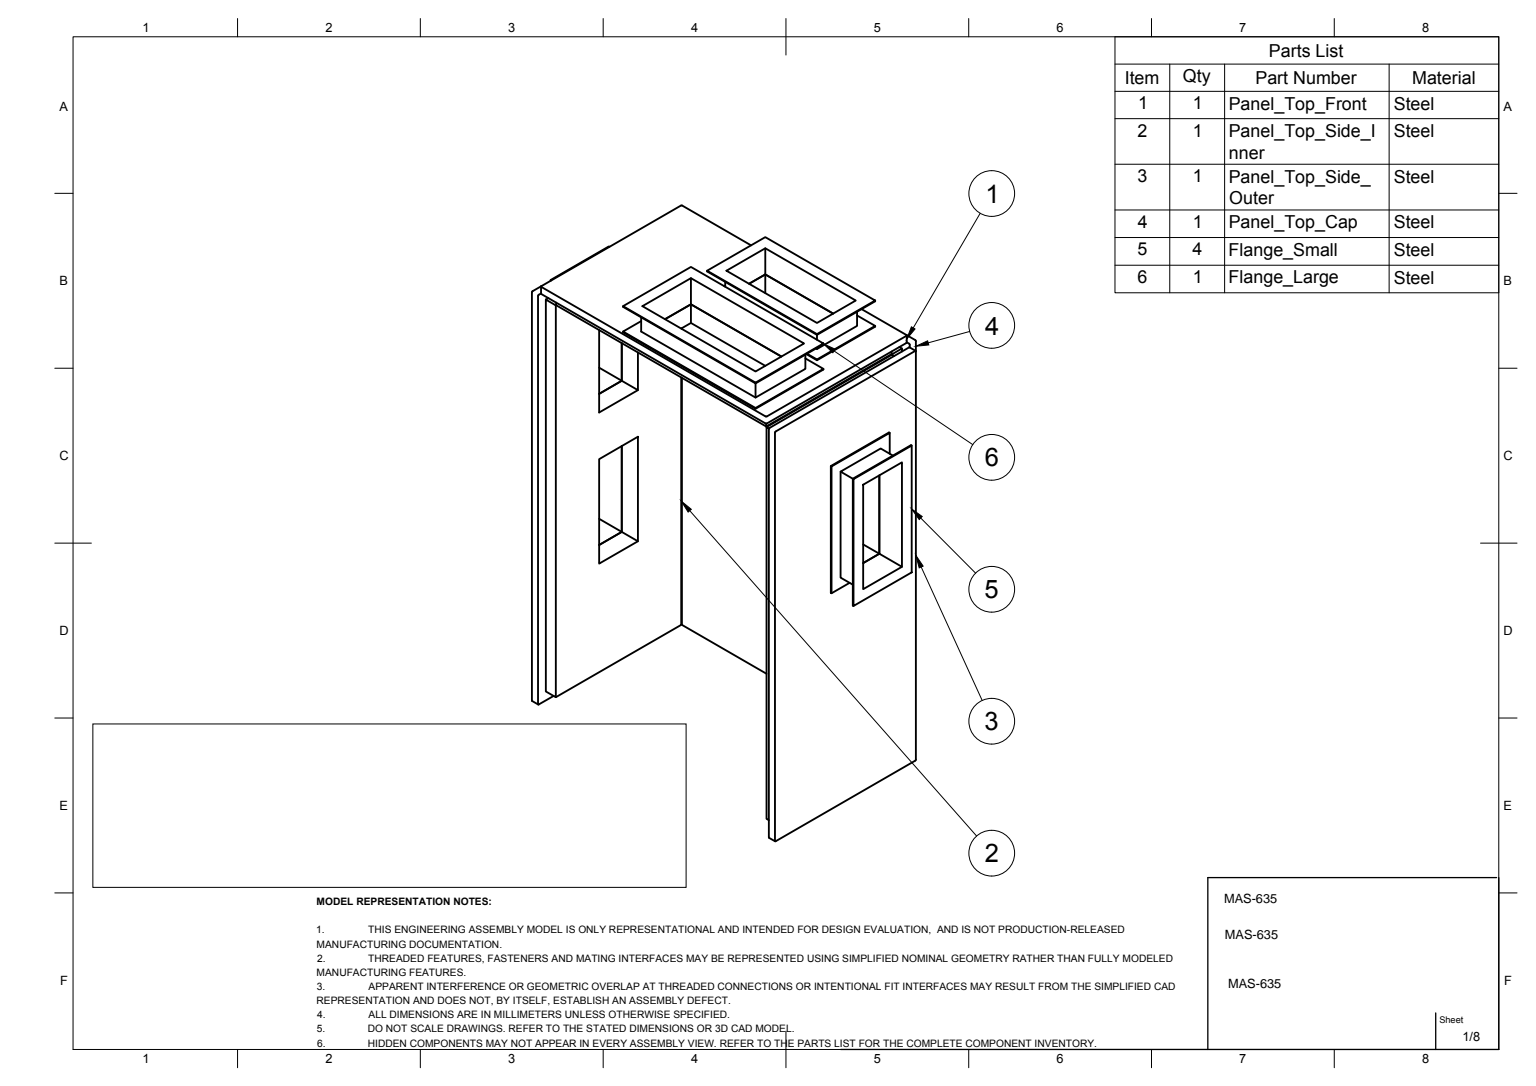
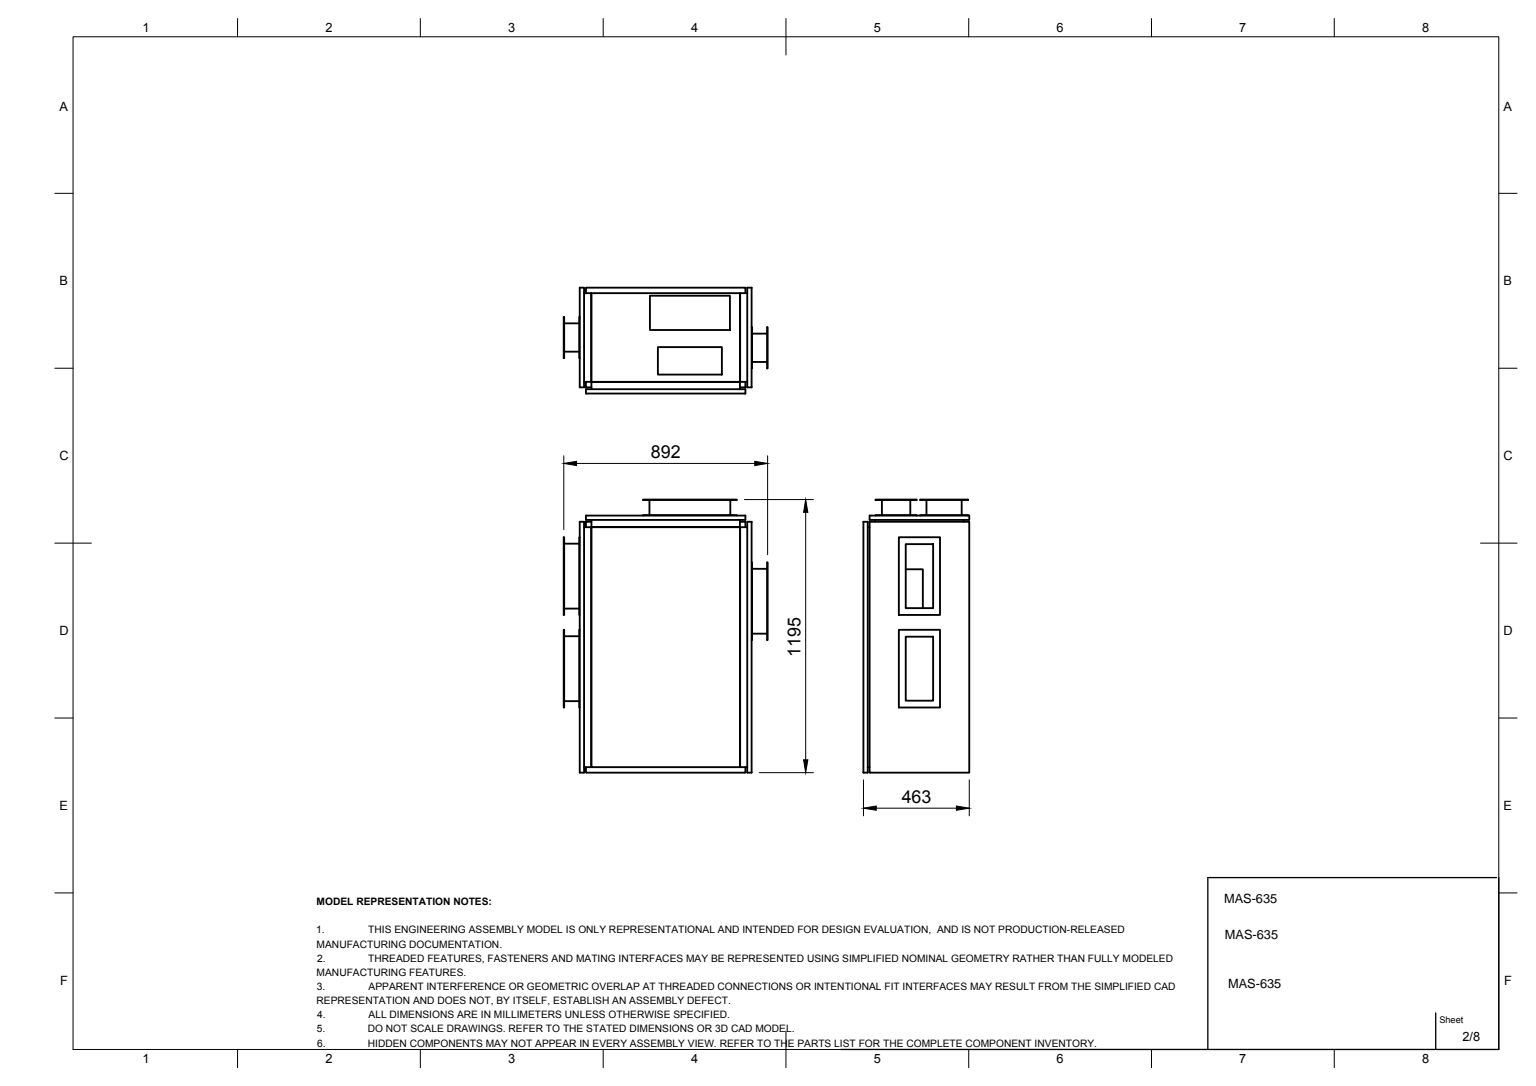
ISO-10303-21;
HEADER;
FILE_DESCRIPTION((''),'2;1');
FILE_NAME('MAS-635','2026-10-09T12:34:24-07:00',(''),(''),'','','');
FILE_SCHEMA (('AUTOMOTIVE_DESIGN { 1 0 10303 214 3 1 1 }'));
ENDSEC;
DATA;
#10 = MECHANICAL_DESIGN_GEOMETRIC_PRESENTATION_REPRESENTATION('',(#59,#60,
#61,#62,#63,#64),#3759) ;
#11 = ITEM_DEFINED_TRANSFORMATION($,$,#2337,#2495) ;
#12 = ITEM_DEFINED_TRANSFORMATION($,$,#2369,#2496) ;
#13 = ITEM_DEFINED_TRANSFORMATION($,$,#2401,#2497) ;
#14 = ITEM_DEFINED_TRANSFORMATION($,$,#2429,#2498) ;
#15 = ITEM_DEFINED_TRANSFORMATION($,$,#2474,#2499) ;
#16 = ITEM_DEFINED_TRANSFORMATION($,$,#2453,#2500) ;
#17 = ITEM_DEFINED_TRANSFORMATION($,$,#2474,#2501) ;
#18 = ITEM_DEFINED_TRANSFORMATION($,$,#2474,#2502) ;
#19 = ITEM_DEFINED_TRANSFORMATION($,$,#2474,#2503) ;
#20 = (
REPRESENTATION_RELATIONSHIP($,$,#3788,#3787)
REPRESENTATION_RELATIONSHIP_WITH_TRANSFORMATION(#11)
SHAPE_REPRESENTATION_RELATIONSHIP()
) ;
#21 = (
REPRESENTATION_RELATIONSHIP($,$,#3789,#3787)
REPRESENTATION_RELATIONSHIP_WITH_TRANSFORMATION(#12)
SHAPE_REPRESENTATION_RELATIONSHIP()
) ;
#22 = (
REPRESENTATION_RELATIONSHIP($,$,#3790,#3787)
REPRESENTATION_RELATIONSHIP_WITH_TRANSFORMATION(#13)
SHAPE_REPRESENTATION_RELATIONSHIP()
) ;
#23 = (
REPRESENTATION_RELATIONSHIP($,$,#3791,#3787)
REPRESENTATION_RELATIONSHIP_WITH_TRANSFORMATION(#14)
SHAPE_REPRESENTATION_RELATIONSHIP()
) ;
#24 = (
REPRESENTATION_RELATIONSHIP($,$,#3793,#3787)
REPRESENTATION_RELATIONSHIP_WITH_TRANSFORMATION(#15)
SHAPE_REPRESENTATION_RELATIONSHIP()
) ;
#25 = (
REPRESENTATION_RELATIONSHIP($,$,#3792,#3787)
REPRESENTATION_RELATIONSHIP_WITH_TRANSFORMATION(#16)
SHAPE_REPRESENTATION_RELATIONSHIP()
) ;
#26 = (
REPRESENTATION_RELATIONSHIP($,$,#3793,#3787)
REPRESENTATION_RELATIONSHIP_WITH_TRANSFORMATION(#17)
SHAPE_REPRESENTATION_RELATIONSHIP()
) ;
#27 = (
REPRESENTATION_RELATIONSHIP($,$,#3793,#3787)
REPRESENTATION_RELATIONSHIP_WITH_TRANSFORMATION(#18)
SHAPE_REPRESENTATION_RELATIONSHIP()
) ;
#28 = (
REPRESENTATION_RELATIONSHIP($,$,#3793,#3787)
REPRESENTATION_RELATIONSHIP_WITH_TRANSFORMATION(#19)
SHAPE_REPRESENTATION_RELATIONSHIP()
) ;
#29 = CONTEXT_DEPENDENT_SHAPE_REPRESENTATION(#20,#3778) ;
#30 = CONTEXT_DEPENDENT_SHAPE_REPRESENTATION(#21,#3779) ;
#31 = CONTEXT_DEPENDENT_SHAPE_REPRESENTATION(#22,#3780) ;
#32 = CONTEXT_DEPENDENT_SHAPE_REPRESENTATION(#23,#3781) ;
#33 = CONTEXT_DEPENDENT_SHAPE_REPRESENTATION(#24,#3782) ;
#34 = CONTEXT_DEPENDENT_SHAPE_REPRESENTATION(#25,#3783) ;
#35 = CONTEXT_DEPENDENT_SHAPE_REPRESENTATION(#26,#3784) ;
#36 = CONTEXT_DEPENDENT_SHAPE_REPRESENTATION(#27,#3785) ;
#37 = CONTEXT_DEPENDENT_SHAPE_REPRESENTATION(#28,#3786) ;
#38 = NEXT_ASSEMBLY_USAGE_OCCURRENCE('Panel_Top_Front:1',
'Panel_Top_Front:1','Panel_Top_Front:1',#3795,#3796,'Panel_Top_Front:1') ;
#39 = NEXT_ASSEMBLY_USAGE_OCCURRENCE('Panel_Top_Side_Inner:1',
'Panel_Top_Side_Inner:1','Panel_Top_Side_Inner:1',#3795,#3797,
'Panel_Top_Side_Inner:1') ;
#40 = NEXT_ASSEMBLY_USAGE_OCCURRENCE('Panel_Top_Side_Outer:1',
'Panel_Top_Side_Outer:1','Panel_Top_Side_Outer:1',#3795,#3798,
'Panel_Top_Side_Outer:1') ;
#41 = NEXT_ASSEMBLY_USAGE_OCCURRENCE('Panel_Top_Cap:1','Panel_Top_Cap:1',
'Panel_Top_Cap:1',#3795,#3799,'Panel_Top_Cap:1') ;
#42 = NEXT_ASSEMBLY_USAGE_OCCURRENCE('Flange_Small:1','Flange_Small:1',
'Flange_Small:1',#3795,#3801,'Flange_Small:1') ;
#43 = NEXT_ASSEMBLY_USAGE_OCCURRENCE('Flange_Large:1','Flange_Large:1',
'Flange_Large:1',#3795,#3800,'Flange_Large:1') ;
#44 = NEXT_ASSEMBLY_USAGE_OCCURRENCE('Flange_Small:2','Flange_Small:2',
'Flange_Small:2',#3795,#3801,'Flange_Small:2') ;
#45 = NEXT_ASSEMBLY_USAGE_OCCURRENCE('Flange_Small:3','Flange_Small:3',
'Flange_Small:3',#3795,#3801,'Flange_Small:3') ;
#46 = NEXT_ASSEMBLY_USAGE_OCCURRENCE('Flange_Small:4','Flange_Small:4',
'Flange_Small:4',#3795,#3801,'Flange_Small:4') ;
#47 = SHAPE_REPRESENTATION_RELATIONSHIP('SRR','None',#3788,#53) ;
#48 = SHAPE_REPRESENTATION_RELATIONSHIP('SRR','None',#3789,#54) ;
#49 = SHAPE_REPRESENTATION_RELATIONSHIP('SRR','None',#3790,#55) ;
#50 = SHAPE_REPRESENTATION_RELATIONSHIP('SRR','None',#3791,#56) ;
#51 = SHAPE_REPRESENTATION_RELATIONSHIP('SRR','None',#3792,#57) ;
#52 = SHAPE_REPRESENTATION_RELATIONSHIP('SRR','None',#3793,#58) ;
#53 = ADVANCED_BREP_SHAPE_REPRESENTATION('',(#65),#3753) ;
#54 = ADVANCED_BREP_SHAPE_REPRESENTATION('',(#66),#3754) ;
#55 = ADVANCED_BREP_SHAPE_REPRESENTATION('',(#67),#3755) ;
#56 = ADVANCED_BREP_SHAPE_REPRESENTATION('',(#68),#3756) ;
#57 = ADVANCED_BREP_SHAPE_REPRESENTATION('',(#69),#3757) ;
#58 = ADVANCED_BREP_SHAPE_REPRESENTATION('',(#70),#3758) ;
#59 = STYLED_ITEM('',(#3827),#65) ;
#60 = STYLED_ITEM('',(#3827),#66) ;
#61 = STYLED_ITEM('',(#3827),#67) ;
#62 = STYLED_ITEM('',(#3827),#68) ;
#63 = STYLED_ITEM('',(#3827),#69) ;
#64 = STYLED_ITEM('',(#3827),#70) ;
#65 = MANIFOLD_SOLID_BREP('Body1',#2263) ;
#66 = MANIFOLD_SOLID_BREP('Body1',#2264) ;
#67 = MANIFOLD_SOLID_BREP('Body1',#2265) ;
#68 = MANIFOLD_SOLID_BREP('Body1',#2266) ;
#69 = MANIFOLD_SOLID_BREP('Body1',#2267) ;
#70 = MANIFOLD_SOLID_BREP('Body1',#2268) ;
#71 = CYLINDRICAL_SURFACE('',#2357,0.2) ;
#72 = CYLINDRICAL_SURFACE('',#2358,0.2) ;
#73 = CYLINDRICAL_SURFACE('',#2359,0.2) ;
#74 = CYLINDRICAL_SURFACE('',#2360,0.2) ;
#75 = CYLINDRICAL_SURFACE('',#2389,0.2) ;
#76 = CYLINDRICAL_SURFACE('',#2390,0.2) ;
#77 = CYLINDRICAL_SURFACE('',#2391,0.2) ;
#78 = CYLINDRICAL_SURFACE('',#2392,0.2) ;
#79 = CYLINDRICAL_SURFACE('',#2421,0.2) ;
#80 = CYLINDRICAL_SURFACE('',#2422,0.2) ;
#81 = CYLINDRICAL_SURFACE('',#2423,0.2) ;
#82 = CYLINDRICAL_SURFACE('',#2424,0.2) ;
#83 = CYLINDRICAL_SURFACE('',#2449,0.2) ;
#84 = CYLINDRICAL_SURFACE('',#2450,0.2) ;
#85 = CYLINDRICAL_SURFACE('',#2451,0.2) ;
#86 = CYLINDRICAL_SURFACE('',#2452,0.2) ;
#87 = CIRCLE('',#2348,0.2) ;
#88 = CIRCLE('',#2349,0.2) ;
#89 = CIRCLE('',#2350,0.2) ;
#90 = CIRCLE('',#2351,0.2) ;
#91 = CIRCLE('',#2353,0.2) ;
#92 = CIRCLE('',#2354,0.2) ;
#93 = CIRCLE('',#2355,0.2) ;
#94 = CIRCLE('',#2356,0.2) ;
#95 = CIRCLE('',#2380,0.2) ;
#96 = CIRCLE('',#2381,0.2) ;
#97 = CIRCLE('',#2382,0.2) ;
#98 = CIRCLE('',#2383,0.2) ;
#99 = CIRCLE('',#2385,0.2) ;
#100 = CIRCLE('',#2386,0.2) ;
#101 = CIRCLE('',#2387,0.2) ;
#102 = CIRCLE('',#2388,0.2) ;
#103 = CIRCLE('',#2412,0.2) ;
#104 = CIRCLE('',#2413,0.2) ;
#105 = CIRCLE('',#2414,0.2) ;
#106 = CIRCLE('',#2415,0.2) ;
#107 = CIRCLE('',#2417,0.2) ;
#108 = CIRCLE('',#2418,0.2) ;
#109 = CIRCLE('',#2419,0.2) ;
#110 = CIRCLE('',#2420,0.2) ;
#111 = CIRCLE('',#2440,0.2) ;
#112 = CIRCLE('',#2441,0.2) ;
#113 = CIRCLE('',#2442,0.2) ;
#114 = CIRCLE('',#2443,0.2) ;
#115 = CIRCLE('',#2445,0.2) ;
#116 = CIRCLE('',#2446,0.2) ;
#117 = CIRCLE('',#2447,0.2) ;
#118 = CIRCLE('',#2448,0.2) ;
#119 = FACE_BOUND('',#266,.T.) ;
#120 = FACE_BOUND('',#267,.T.) ;
#121 = FACE_BOUND('',#273,.T.) ;
#122 = FACE_BOUND('',#275,.T.) ;
#123 = FACE_BOUND('',#276,.T.) ;
#124 = FACE_BOUND('',#294,.T.) ;
#125 = FACE_BOUND('',#295,.T.) ;
#126 = FACE_BOUND('',#301,.T.) ;
#127 = FACE_BOUND('',#303,.T.) ;
#128 = FACE_BOUND('',#304,.T.) ;
#129 = FACE_BOUND('',#322,.T.) ;
#130 = FACE_BOUND('',#328,.T.) ;
#131 = FACE_BOUND('',#330,.T.) ;
#132 = FACE_BOUND('',#349,.T.) ;
#133 = FACE_BOUND('',#360,.T.) ;
#134 = FACE_BOUND('',#362,.T.) ;
#135 = FACE_BOUND('',#372,.T.) ;
#136 = FACE_BOUND('',#374,.T.) ;
#137 = FACE_BOUND('',#384,.T.) ;
#138 = FACE_BOUND('',#386,.T.) ;
#139 = FACE_BOUND('',#396,.T.) ;
#140 = FACE_BOUND('',#398,.T.) ;
#141 = FACE_OUTER_BOUND('',#261,.T.) ;
#142 = FACE_OUTER_BOUND('',#262,.T.) ;
#143 = FACE_OUTER_BOUND('',#263,.T.) ;
#144 = FACE_OUTER_BOUND('',#264,.T.) ;
#145 = FACE_OUTER_BOUND('',#265,.T.) ;
#146 = FACE_OUTER_BOUND('',#268,.T.) ;
#147 = FACE_OUTER_BOUND('',#269,.T.) ;
#148 = FACE_OUTER_BOUND('',#270,.T.) ;
#149 = FACE_OUTER_BOUND('',#271,.T.) ;
#150 = FACE_OUTER_BOUND('',#272,.T.) ;
#151 = FACE_OUTER_BOUND('',#274,.T.) ;
#152 = FACE_OUTER_BOUND('',#277,.T.) ;
#153 = FACE_OUTER_BOUND('',#278,.T.) ;
#154 = FACE_OUTER_BOUND('',#279,.T.) ;
#155 = FACE_OUTER_BOUND('',#280,.T.) ;
#156 = FACE_OUTER_BOUND('',#281,.T.) ;
#157 = FACE_OUTER_BOUND('',#282,.T.) ;
#158 = FACE_OUTER_BOUND('',#283,.T.) ;
#159 = FACE_OUTER_BOUND('',#284,.T.) ;
#160 = FACE_OUTER_BOUND('',#285,.T.) ;
#161 = FACE_OUTER_BOUND('',#286,.T.) ;
#162 = FACE_OUTER_BOUND('',#287,.T.) ;
#163 = FACE_OUTER_BOUND('',#288,.T.) ;
#164 = FACE_OUTER_BOUND('',#289,.T.) ;
#165 = FACE_OUTER_BOUND('',#290,.T.) ;
#166 = FACE_OUTER_BOUND('',#291,.T.) ;
#167 = FACE_OUTER_BOUND('',#292,.T.) ;
#168 = FACE_OUTER_BOUND('',#293,.T.) ;
#169 = FACE_OUTER_BOUND('',#296,.T.) ;
#170 = FACE_OUTER_BOUND('',#297,.T.) ;
#171 = FACE_OUTER_BOUND('',#298,.T.) ;
#172 = FACE_OUTER_BOUND('',#299,.T.) ;
#173 = FACE_OUTER_BOUND('',#300,.T.) ;
#174 = FACE_OUTER_BOUND('',#302,.T.) ;
#175 = FACE_OUTER_BOUND('',#305,.T.) ;
#176 = FACE_OUTER_BOUND('',#306,.T.) ;
#177 = FACE_OUTER_BOUND('',#307,.T.) ;
#178 = FACE_OUTER_BOUND('',#308,.T.) ;
#179 = FACE_OUTER_BOUND('',#309,.T.) ;
#180 = FACE_OUTER_BOUND('',#310,.T.) ;
#181 = FACE_OUTER_BOUND('',#311,.T.) ;
#182 = FACE_OUTER_BOUND('',#312,.T.) ;
#183 = FACE_OUTER_BOUND('',#313,.T.) ;
#184 = FACE_OUTER_BOUND('',#314,.T.) ;
#185 = FACE_OUTER_BOUND('',#315,.T.) ;
#186 = FACE_OUTER_BOUND('',#316,.T.) ;
#187 = FACE_OUTER_BOUND('',#317,.T.) ;
#188 = FACE_OUTER_BOUND('',#318,.T.) ;
#189 = FACE_OUTER_BOUND('',#319,.T.) ;
#190 = FACE_OUTER_BOUND('',#320,.T.) ;
#191 = FACE_OUTER_BOUND('',#321,.T.) ;
#192 = FACE_OUTER_BOUND('',#323,.T.) ;
#193 = FACE_OUTER_BOUND('',#324,.T.) ;
#194 = FACE_OUTER_BOUND('',#325,.T.) ;
#195 = FACE_OUTER_BOUND('',#326,.T.) ;
#196 = FACE_OUTER_BOUND('',#327,.T.) ;
#197 = FACE_OUTER_BOUND('',#329,.T.) ;
#198 = FACE_OUTER_BOUND('',#331,.T.) ;
#199 = FACE_OUTER_BOUND('',#332,.T.) ;
#200 = FACE_OUTER_BOUND('',#333,.T.) ;
#201 = FACE_OUTER_BOUND('',#334,.T.) ;
#202 = FACE_OUTER_BOUND('',#335,.T.) ;
#203 = FACE_OUTER_BOUND('',#336,.T.) ;
#204 = FACE_OUTER_BOUND('',#337,.T.) ;
#205 = FACE_OUTER_BOUND('',#338,.T.) ;
#206 = FACE_OUTER_BOUND('',#339,.T.) ;
#207 = FACE_OUTER_BOUND('',#340,.T.) ;
#208 = FACE_OUTER_BOUND('',#341,.T.) ;
#209 = FACE_OUTER_BOUND('',#342,.T.) ;
#210 = FACE_OUTER_BOUND('',#343,.T.) ;
#211 = FACE_OUTER_BOUND('',#344,.T.) ;
#212 = FACE_OUTER_BOUND('',#345,.T.) ;
#213 = FACE_OUTER_BOUND('',#346,.T.) ;
#214 = FACE_OUTER_BOUND('',#347,.T.) ;
#215 = FACE_OUTER_BOUND('',#348,.T.) ;
#216 = FACE_OUTER_BOUND('',#350,.T.) ;
#217 = FACE_OUTER_BOUND('',#351,.T.) ;
#218 = FACE_OUTER_BOUND('',#352,.T.) ;
#219 = FACE_OUTER_BOUND('',#353,.T.) ;
#220 = FACE_OUTER_BOUND('',#354,.T.) ;
#221 = FACE_OUTER_BOUND('',#355,.T.) ;
#222 = FACE_OUTER_BOUND('',#356,.T.) ;
#223 = FACE_OUTER_BOUND('',#357,.T.) ;
#224 = FACE_OUTER_BOUND('',#358,.T.) ;
#225 = FACE_OUTER_BOUND('',#359,.T.) ;
#226 = FACE_OUTER_BOUND('',#361,.T.) ;
#227 = FACE_OUTER_BOUND('',#363,.T.) ;
#228 = FACE_OUTER_BOUND('',#364,.T.) ;
#229 = FACE_OUTER_BOUND('',#365,.T.) ;
#230 = FACE_OUTER_BOUND('',#366,.T.) ;
#231 = FACE_OUTER_BOUND('',#367,.T.) ;
#232 = FACE_OUTER_BOUND('',#368,.T.) ;
#233 = FACE_OUTER_BOUND('',#369,.T.) ;
#234 = FACE_OUTER_BOUND('',#370,.T.) ;
#235 = FACE_OUTER_BOUND('',#371,.T.) ;
#236 = FACE_OUTER_BOUND('',#373,.T.) ;
#237 = FACE_OUTER_BOUND('',#375,.T.) ;
#238 = FACE_OUTER_BOUND('',#376,.T.) ;
#239 = FACE_OUTER_BOUND('',#377,.T.) ;
#240 = FACE_OUTER_BOUND('',#378,.T.) ;
#241 = FACE_OUTER_BOUND('',#379,.T.) ;
#242 = FACE_OUTER_BOUND('',#380,.T.) ;
#243 = FACE_OUTER_BOUND('',#381,.T.) ;
#244 = FACE_OUTER_BOUND('',#382,.T.) ;
#245 = FACE_OUTER_BOUND('',#383,.T.) ;
#246 = FACE_OUTER_BOUND('',#385,.T.) ;
#247 = FACE_OUTER_BOUND('',#387,.T.) ;
#248 = FACE_OUTER_BOUND('',#388,.T.) ;
#249 = FACE_OUTER_BOUND('',#389,.T.) ;
#250 = FACE_OUTER_BOUND('',#390,.T.) ;
#251 = FACE_OUTER_BOUND('',#391,.T.) ;
#252 = FACE_OUTER_BOUND('',#392,.T.) ;
#253 = FACE_OUTER_BOUND('',#393,.T.) ;
#254 = FACE_OUTER_BOUND('',#394,.T.) ;
#255 = FACE_OUTER_BOUND('',#395,.T.) ;
#256 = FACE_OUTER_BOUND('',#397,.T.) ;
#257 = FACE_OUTER_BOUND('',#399,.T.) ;
#258 = FACE_OUTER_BOUND('',#400,.T.) ;
#259 = FACE_OUTER_BOUND('',#401,.T.) ;
#260 = FACE_OUTER_BOUND('',#402,.T.) ;
#261 = EDGE_LOOP('',(#1439,#1440,#1441,#1442)) ;
#262 = EDGE_LOOP('',(#1443,#1444,#1445,#1446)) ;
#263 = EDGE_LOOP('',(#1447,#1448,#1449,#1450)) ;
#264 = EDGE_LOOP('',(#1451,#1452,#1453,#1454)) ;
#265 = EDGE_LOOP('',(#1455,#1456,#1457,#1458)) ;
#266 = EDGE_LOOP('',(#1459,#1460,#1461,#1462)) ;
#267 = EDGE_LOOP('',(#1463,#1464,#1465,#1466)) ;
#268 = EDGE_LOOP('',(#1467,#1468,#1469,#1470)) ;
#269 = EDGE_LOOP('',(#1471,#1472,#1473,#1474)) ;
#270 = EDGE_LOOP('',(#1475,#1476,#1477,#1478)) ;
#271 = EDGE_LOOP('',(#1479,#1480,#1481,#1482)) ;
#272 = EDGE_LOOP('',(#1483,#1484,#1485,#1486,#1487,#1488,#1489,#1490)) ;
#273 = EDGE_LOOP('',(#1491,#1492,#1493,#1494)) ;
#274 = EDGE_LOOP('',(#1495,#1496,#1497,#1498,#1499,#1500,#1501,#1502)) ;
#275 = EDGE_LOOP('',(#1503,#1504,#1505,#1506)) ;
#276 = EDGE_LOOP('',(#1507,#1508,#1509,#1510)) ;
#277 = EDGE_LOOP('',(#1511,#1512,#1513,#1514)) ;
#278 = EDGE_LOOP('',(#1515,#1516,#1517,#1518)) ;
#279 = EDGE_LOOP('',(#1519,#1520,#1521,#1522)) ;
#280 = EDGE_LOOP('',(#1523,#1524,#1525,#1526)) ;
#281 = EDGE_LOOP('',(#1527,#1528,#1529,#1530)) ;
#282 = EDGE_LOOP('',(#1531,#1532,#1533,#1534)) ;
#283 = EDGE_LOOP('',(#1535,#1536,#1537,#1538)) ;
#284 = EDGE_LOOP('',(#1539,#1540,#1541,#1542)) ;
#285 = EDGE_LOOP('',(#1543,#1544,#1545,#1546)) ;
#286 = EDGE_LOOP('',(#1547,#1548,#1549,#1550)) ;
#287 = EDGE_LOOP('',(#1551,#1552,#1553,#1554)) ;
#288 = EDGE_LOOP('',(#1555,#1556,#1557,#1558)) ;
#289 = EDGE_LOOP('',(#1559,#1560,#1561,#1562)) ;
#290 = EDGE_LOOP('',(#1563,#1564,#1565,#1566)) ;
#291 = EDGE_LOOP('',(#1567,#1568,#1569,#1570)) ;
#292 = EDGE_LOOP('',(#1571,#1572,#1573,#1574)) ;
#293 = EDGE_LOOP('',(#1575,#1576,#1577,#1578)) ;
#294 = EDGE_LOOP('',(#1579,#1580,#1581,#1582)) ;
#295 = EDGE_LOOP('',(#1583,#1584,#1585,#1586)) ;
#296 = EDGE_LOOP('',(#1587,#1588,#1589,#1590)) ;
#297 = EDGE_LOOP('',(#1591,#1592,#1593,#1594)) ;
#298 = EDGE_LOOP('',(#1595,#1596,#1597,#1598)) ;
#299 = EDGE_LOOP('',(#1599,#1600,#1601,#1602)) ;
#300 = EDGE_LOOP('',(#1603,#1604,#1605,#1606,#1607,#1608,#1609,#1610)) ;
#301 = EDGE_LOOP('',(#1611,#1612,#1613,#1614)) ;
#302 = EDGE_LOOP('',(#1615,#1616,#1617,#1618,#1619,#1620,#1621,#1622)) ;
#303 = EDGE_LOOP('',(#1623,#1624,#1625,#1626)) ;
#304 = EDGE_LOOP('',(#1627,#1628,#1629,#1630)) ;
#305 = EDGE_LOOP('',(#1631,#1632,#1633,#1634)) ;
#306 = EDGE_LOOP('',(#1635,#1636,#1637,#1638)) ;
#307 = EDGE_LOOP('',(#1639,#1640,#1641,#1642)) ;
#308 = EDGE_LOOP('',(#1643,#1644,#1645,#1646)) ;
#309 = EDGE_LOOP('',(#1647,#1648,#1649,#1650)) ;
#310 = EDGE_LOOP('',(#1651,#1652,#1653,#1654)) ;
#311 = EDGE_LOOP('',(#1655,#1656,#1657,#1658)) ;
#312 = EDGE_LOOP('',(#1659,#1660,#1661,#1662)) ;
#313 = EDGE_LOOP('',(#1663,#1664,#1665,#1666)) ;
#314 = EDGE_LOOP('',(#1667,#1668,#1669,#1670)) ;
#315 = EDGE_LOOP('',(#1671,#1672,#1673,#1674)) ;
#316 = EDGE_LOOP('',(#1675,#1676,#1677,#1678)) ;
#317 = EDGE_LOOP('',(#1679,#1680,#1681,#1682)) ;
#318 = EDGE_LOOP('',(#1683,#1684,#1685,#1686)) ;
#319 = EDGE_LOOP('',(#1687,#1688,#1689,#1690)) ;
#320 = EDGE_LOOP('',(#1691,#1692,#1693,#1694)) ;
#321 = EDGE_LOOP('',(#1695,#1696,#1697,#1698)) ;
#322 = EDGE_LOOP('',(#1699,#1700,#1701,#1702)) ;
#323 = EDGE_LOOP('',(#1703,#1704,#1705,#1706)) ;
#324 = EDGE_LOOP('',(#1707,#1708,#1709,#1710)) ;
#325 = EDGE_LOOP('',(#1711,#1712,#1713,#1714)) ;
#326 = EDGE_LOOP('',(#1715,#1716,#1717,#1718)) ;
#327 = EDGE_LOOP('',(#1719,#1720,#1721,#1722,#1723,#1724,#1725,#1726)) ;
#328 = EDGE_LOOP('',(#1727,#1728,#1729,#1730)) ;
#329 = EDGE_LOOP('',(#1731,#1732,#1733,#1734,#1735,#1736,#1737,#1738)) ;
#330 = EDGE_LOOP('',(#1739,#1740,#1741,#1742)) ;
#331 = EDGE_LOOP('',(#1743,#1744,#1745,#1746)) ;
#332 = EDGE_LOOP('',(#1747,#1748,#1749,#1750)) ;
#333 = EDGE_LOOP('',(#1751,#1752,#1753,#1754)) ;
#334 = EDGE_LOOP('',(#1755,#1756,#1757,#1758)) ;
#335 = EDGE_LOOP('',(#1759,#1760,#1761,#1762)) ;
#336 = EDGE_LOOP('',(#1763,#1764,#1765,#1766)) ;
#337 = EDGE_LOOP('',(#1767,#1768,#1769,#1770)) ;
#338 = EDGE_LOOP('',(#1771,#1772,#1773,#1774)) ;
#339 = EDGE_LOOP('',(#1775,#1776,#1777,#1778)) ;
#340 = EDGE_LOOP('',(#1779,#1780,#1781,#1782)) ;
#341 = EDGE_LOOP('',(#1783,#1784,#1785,#1786)) ;
#342 = EDGE_LOOP('',(#1787,#1788,#1789,#1790)) ;
#343 = EDGE_LOOP('',(#1791,#1792,#1793,#1794)) ;
#344 = EDGE_LOOP('',(#1795,#1796,#1797,#1798)) ;
#345 = EDGE_LOOP('',(#1799,#1800,#1801,#1802)) ;
#346 = EDGE_LOOP('',(#1803,#1804,#1805,#1806)) ;
#347 = EDGE_LOOP('',(#1807,#1808,#1809,#1810)) ;
#348 = EDGE_LOOP('',(#1811,#1812,#1813,#1814,#1815,#1816,#1817,#1818)) ;
#349 = EDGE_LOOP('',(#1819,#1820,#1821,#1822)) ;
#350 = EDGE_LOOP('',(#1823,#1824,#1825,#1826,#1827,#1828,#1829,#1830)) ;
#351 = EDGE_LOOP('',(#1831,#1832,#1833,#1834)) ;
#352 = EDGE_LOOP('',(#1835,#1836,#1837,#1838)) ;
#353 = EDGE_LOOP('',(#1839,#1840,#1841,#1842)) ;
#354 = EDGE_LOOP('',(#1843,#1844,#1845,#1846)) ;
#355 = EDGE_LOOP('',(#1847,#1848,#1849,#1850)) ;
#356 = EDGE_LOOP('',(#1851,#1852,#1853,#1854)) ;
#357 = EDGE_LOOP('',(#1855,#1856,#1857,#1858)) ;
#358 = EDGE_LOOP('',(#1859,#1860,#1861,#1862)) ;
#359 = EDGE_LOOP('',(#1863,#1864,#1865,#1866)) ;
#360 = EDGE_LOOP('',(#1867,#1868,#1869,#1870)) ;
#361 = EDGE_LOOP('',(#1871,#1872,#1873,#1874)) ;
#362 = EDGE_LOOP('',(#1875,#1876,#1877,#1878)) ;
#363 = EDGE_LOOP('',(#1879,#1880,#1881,#1882)) ;
#364 = EDGE_LOOP('',(#1883,#1884,#1885,#1886)) ;
#365 = EDGE_LOOP('',(#1887,#1888,#1889,#1890)) ;
#366 = EDGE_LOOP('',(#1891,#1892,#1893,#1894)) ;
#367 = EDGE_LOOP('',(#1895,#1896,#1897,#1898)) ;
#368 = EDGE_LOOP('',(#1899,#1900,#1901,#1902)) ;
#369 = EDGE_LOOP('',(#1903,#1904,#1905,#1906)) ;
#370 = EDGE_LOOP('',(#1907,#1908,#1909,#1910)) ;
#371 = EDGE_LOOP('',(#1911,#1912,#1913,#1914)) ;
#372 = EDGE_LOOP('',(#1915,#1916,#1917,#1918)) ;
#373 = EDGE_LOOP('',(#1919,#1920,#1921,#1922)) ;
#374 = EDGE_LOOP('',(#1923,#1924,#1925,#1926)) ;
#375 = EDGE_LOOP('',(#1927,#1928,#1929,#1930)) ;
#376 = EDGE_LOOP('',(#1931,#1932,#1933,#1934)) ;
#377 = EDGE_LOOP('',(#1935,#1936,#1937,#1938)) ;
#378 = EDGE_LOOP('',(#1939,#1940,#1941,#1942)) ;
#379 = EDGE_LOOP('',(#1943,#1944,#1945,#1946)) ;
#380 = EDGE_LOOP('',(#1947,#1948,#1949,#1950)) ;
#381 = EDGE_LOOP('',(#1951,#1952,#1953,#1954)) ;
#382 = EDGE_LOOP('',(#1955,#1956,#1957,#1958)) ;
#383 = EDGE_LOOP('',(#1959,#1960,#1961,#1962)) ;
#384 = EDGE_LOOP('',(#1963,#1964,#1965,#1966)) ;
#385 = EDGE_LOOP('',(#1967,#1968,#1969,#1970)) ;
#386 = EDGE_LOOP('',(#1971,#1972,#1973,#1974)) ;
#387 = EDGE_LOOP('',(#1975,#1976,#1977,#1978)) ;
#388 = EDGE_LOOP('',(#1979,#1980,#1981,#1982)) ;
#389 = EDGE_LOOP('',(#1983,#1984,#1985,#1986)) ;
#390 = EDGE_LOOP('',(#1987,#1988,#1989,#1990)) ;
#391 = EDGE_LOOP('',(#1991,#1992,#1993,#1994)) ;
#392 = EDGE_LOOP('',(#1995,#1996,#1997,#1998)) ;
#393 = EDGE_LOOP('',(#1999,#2000,#2001,#2002)) ;
#394 = EDGE_LOOP('',(#2003,#2004,#2005,#2006)) ;
#395 = EDGE_LOOP('',(#2007,#2008,#2009,#2010)) ;
#396 = EDGE_LOOP('',(#2011,#2012,#2013,#2014)) ;
#397 = EDGE_LOOP('',(#2015,#2016,#2017,#2018)) ;
#398 = EDGE_LOOP('',(#2019,#2020,#2021,#2022)) ;
#399 = EDGE_LOOP('',(#2023,#2024,#2025,#2026)) ;
#400 = EDGE_LOOP('',(#2027,#2028,#2029,#2030)) ;
#401 = EDGE_LOOP('',(#2031,#2032,#2033,#2034)) ;
#402 = EDGE_LOOP('',(#2035,#2036,#2037,#2038)) ;
#403 = LINE('',#3113,#671) ;
#404 = LINE('',#3115,#672) ;
#405 = LINE('',#3117,#673) ;
#406 = LINE('',#3118,#674) ;
#407 = LINE('',#3121,#675) ;
#408 = LINE('',#3123,#676) ;
#409 = LINE('',#3124,#677) ;
#410 = LINE('',#3127,#678) ;
#411 = LINE('',#3129,#679) ;
#412 = LINE('',#3130,#680) ;
#413 = LINE('',#3132,#681) ;
#414 = LINE('',#3133,#682) ;
#415 = LINE('',#3137,#683) ;
#416 = LINE('',#3139,#684) ;
#417 = LINE('',#3141,#685) ;
#418 = LINE('',#3142,#686) ;
#419 = LINE('',#3145,#687) ;
#420 = LINE('',#3147,#688) ;
#421 = LINE('',#3149,#689) ;
#422 = LINE('',#3150,#690) ;
#423 = LINE('',#3154,#691) ;
#424 = LINE('',#3156,#692) ;
#425 = LINE('',#3158,#693) ;
#426 = LINE('',#3159,#694) ;
#427 = LINE('',#3163,#695) ;
#428 = LINE('',#3165,#696) ;
#429 = LINE('',#3167,#697) ;
#430 = LINE('',#3168,#698) ;
#431 = LINE('',#3172,#699) ;
#432 = LINE('',#3174,#700) ;
#433 = LINE('',#3176,#701) ;
#434 = LINE('',#3177,#702) ;
#435 = LINE('',#3181,#703) ;
#436 = LINE('',#3183,#704) ;
#437 = LINE('',#3185,#705) ;
#438 = LINE('',#3186,#706) ;
#439 = LINE('',#3199,#707) ;
#440 = LINE('',#3201,#708) ;
#441 = LINE('',#3203,#709) ;
#442 = LINE('',#3204,#710) ;
#443 = LINE('',#3207,#711) ;
#444 = LINE('',#3209,#712) ;
#445 = LINE('',#3211,#713) ;
#446 = LINE('',#3212,#714) ;
#447 = LINE('',#3218,#715) ;
#448 = LINE('',#3219,#716) ;
#449 = LINE('',#3221,#717) ;
#450 = LINE('',#3223,#718) ;
#451 = LINE('',#3226,#719) ;
#452 = LINE('',#3227,#720) ;
#453 = LINE('',#3229,#721) ;
#454 = LINE('',#3231,#722) ;
#455 = LINE('',#3237,#723) ;
#456 = LINE('',#3239,#724) ;
#457 = LINE('',#3241,#725) ;
#458 = LINE('',#3242,#726) ;
#459 = LINE('',#3245,#727) ;
#460 = LINE('',#3247,#728) ;
#461 = LINE('',#3248,#729) ;
#462 = LINE('',#3251,#730) ;
#463 = LINE('',#3253,#731) ;
#464 = LINE('',#3254,#732) ;
#465 = LINE('',#3256,#733) ;
#466 = LINE('',#3257,#734) ;
#467 = LINE('',#3261,#735) ;
#468 = LINE('',#3263,#736) ;
#469 = LINE('',#3265,#737) ;
#470 = LINE('',#3266,#738) ;
#471 = LINE('',#3269,#739) ;
#472 = LINE('',#3271,#740) ;
#473 = LINE('',#3273,#741) ;
#474 = LINE('',#3274,#742) ;
#475 = LINE('',#3278,#743) ;
#476 = LINE('',#3280,#744) ;
#477 = LINE('',#3282,#745) ;
#478 = LINE('',#3283,#746) ;
#479 = LINE('',#3287,#747) ;
#480 = LINE('',#3289,#748) ;
#481 = LINE('',#3291,#749) ;
#482 = LINE('',#3292,#750) ;
#483 = LINE('',#3296,#751) ;
#484 = LINE('',#3298,#752) ;
#485 = LINE('',#3300,#753) ;
#486 = LINE('',#3301,#754) ;
#487 = LINE('',#3305,#755) ;
#488 = LINE('',#3307,#756) ;
#489 = LINE('',#3309,#757) ;
#490 = LINE('',#3310,#758) ;
#491 = LINE('',#3323,#759) ;
#492 = LINE('',#3325,#760) ;
#493 = LINE('',#3327,#761) ;
#494 = LINE('',#3328,#762) ;
#495 = LINE('',#3331,#763) ;
#496 = LINE('',#3333,#764) ;
#497 = LINE('',#3335,#765) ;
#498 = LINE('',#3336,#766) ;
#499 = LINE('',#3342,#767) ;
#500 = LINE('',#3343,#768) ;
#501 = LINE('',#3345,#769) ;
#502 = LINE('',#3347,#770) ;
#503 = LINE('',#3350,#771) ;
#504 = LINE('',#3351,#772) ;
#505 = LINE('',#3353,#773) ;
#506 = LINE('',#3355,#774) ;
#507 = LINE('',#3361,#775) ;
#508 = LINE('',#3363,#776) ;
#509 = LINE('',#3365,#777) ;
#510 = LINE('',#3366,#778) ;
#511 = LINE('',#3369,#779) ;
#512 = LINE('',#3371,#780) ;
#513 = LINE('',#3372,#781) ;
#514 = LINE('',#3375,#782) ;
#515 = LINE('',#3377,#783) ;
#516 = LINE('',#3378,#784) ;
#517 = LINE('',#3380,#785) ;
#518 = LINE('',#3381,#786) ;
#519 = LINE('',#3385,#787) ;
#520 = LINE('',#3387,#788) ;
#521 = LINE('',#3389,#789) ;
#522 = LINE('',#3390,#790) ;
#523 = LINE('',#3394,#791) ;
#524 = LINE('',#3396,#792) ;
#525 = LINE('',#3398,#793) ;
#526 = LINE('',#3399,#794) ;
#527 = LINE('',#3403,#795) ;
#528 = LINE('',#3405,#796) ;
#529 = LINE('',#3407,#797) ;
#530 = LINE('',#3408,#798) ;
#531 = LINE('',#3412,#799) ;
#532 = LINE('',#3414,#800) ;
#533 = LINE('',#3416,#801) ;
#534 = LINE('',#3417,#802) ;
#535 = LINE('',#3421,#803) ;
#536 = LINE('',#3423,#804) ;
#537 = LINE('',#3425,#805) ;
#538 = LINE('',#3426,#806) ;
#539 = LINE('',#3439,#807) ;
#540 = LINE('',#3441,#808) ;
#541 = LINE('',#3443,#809) ;
#542 = LINE('',#3444,#810) ;
#543 = LINE('',#3450,#811) ;
#544 = LINE('',#3451,#812) ;
#545 = LINE('',#3453,#813) ;
#546 = LINE('',#3455,#814) ;
#547 = LINE('',#3461,#815) ;
#548 = LINE('',#3463,#816) ;
#549 = LINE('',#3465,#817) ;
#550 = LINE('',#3466,#818) ;
#551 = LINE('',#3469,#819) ;
#552 = LINE('',#3471,#820) ;
#553 = LINE('',#3472,#821) ;
#554 = LINE('',#3475,#822) ;
#555 = LINE('',#3477,#823) ;
#556 = LINE('',#3478,#824) ;
#557 = LINE('',#3480,#825) ;
#558 = LINE('',#3481,#826) ;
#559 = LINE('',#3486,#827) ;
#560 = LINE('',#3488,#828) ;
#561 = LINE('',#3490,#829) ;
#562 = LINE('',#3491,#830) ;
#563 = LINE('',#3495,#831) ;
#564 = LINE('',#3497,#832) ;
#565 = LINE('',#3499,#833) ;
#566 = LINE('',#3500,#834) ;
#567 = LINE('',#3504,#835) ;
#568 = LINE('',#3506,#836) ;
#569 = LINE('',#3508,#837) ;
#570 = LINE('',#3509,#838) ;
#571 = LINE('',#3513,#839) ;
#572 = LINE('',#3515,#840) ;
#573 = LINE('',#3517,#841) ;
#574 = LINE('',#3518,#842) ;
#575 = LINE('',#3537,#843) ;
#576 = LINE('',#3539,#844) ;
#577 = LINE('',#3541,#845) ;
#578 = LINE('',#3542,#846) ;
#579 = LINE('',#3545,#847) ;
#580 = LINE('',#3547,#848) ;
#581 = LINE('',#3548,#849) ;
#582 = LINE('',#3551,#850) ;
#583 = LINE('',#3553,#851) ;
#584 = LINE('',#3554,#852) ;
#585 = LINE('',#3556,#853) ;
#586 = LINE('',#3557,#854) ;
#587 = LINE('',#3561,#855) ;
#588 = LINE('',#3563,#856) ;
#589 = LINE('',#3565,#857) ;
#590 = LINE('',#3566,#858) ;
#591 = LINE('',#3570,#859) ;
#592 = LINE('',#3572,#860) ;
#593 = LINE('',#3574,#861) ;
#594 = LINE('',#3575,#862) ;
#595 = LINE('',#3578,#863) ;
#596 = LINE('',#3580,#864) ;
#597 = LINE('',#3582,#865) ;
#598 = LINE('',#3583,#866) ;
#599 = LINE('',#3585,#867) ;
#600 = LINE('',#3586,#868) ;
#601 = LINE('',#3588,#869) ;
#602 = LINE('',#3590,#870) ;
#603 = LINE('',#3594,#871) ;
#604 = LINE('',#3596,#872) ;
#605 = LINE('',#3597,#873) ;
#606 = LINE('',#3600,#874) ;
#607 = LINE('',#3601,#875) ;
#608 = LINE('',#3604,#876) ;
#609 = LINE('',#3605,#877) ;
#610 = LINE('',#3607,#878) ;
#611 = LINE('',#3611,#879) ;
#612 = LINE('',#3613,#880) ;
#613 = LINE('',#3615,#881) ;
#614 = LINE('',#3616,#882) ;
#615 = LINE('',#3620,#883) ;
#616 = LINE('',#3622,#884) ;
#617 = LINE('',#3624,#885) ;
#618 = LINE('',#3625,#886) ;
#619 = LINE('',#3627,#887) ;
#620 = LINE('',#3628,#888) ;
#621 = LINE('',#3630,#889) ;
#622 = LINE('',#3632,#890) ;
#623 = LINE('',#3638,#891) ;
#624 = LINE('',#3640,#892) ;
#625 = LINE('',#3642,#893) ;
#626 = LINE('',#3643,#894) ;
#627 = LINE('',#3646,#895) ;
#628 = LINE('',#3648,#896) ;
#629 = LINE('',#3649,#897) ;
#630 = LINE('',#3652,#898) ;
#631 = LINE('',#3654,#899) ;
#632 = LINE('',#3655,#900) ;
#633 = LINE('',#3657,#901) ;
#634 = LINE('',#3658,#902) ;
#635 = LINE('',#3662,#903) ;
#636 = LINE('',#3664,#904) ;
#637 = LINE('',#3666,#905) ;
#638 = LINE('',#3667,#906) ;
#639 = LINE('',#3671,#907) ;
#640 = LINE('',#3673,#908) ;
#641 = LINE('',#3675,#909) ;
#642 = LINE('',#3676,#910) ;
#643 = LINE('',#3679,#911) ;
#644 = LINE('',#3681,#912) ;
#645 = LINE('',#3683,#913) ;
#646 = LINE('',#3684,#914) ;
#647 = LINE('',#3686,#915) ;
#648 = LINE('',#3687,#916) ;
#649 = LINE('',#3689,#917) ;
#650 = LINE('',#3691,#918) ;
#651 = LINE('',#3695,#919) ;
#652 = LINE('',#3697,#920) ;
#653 = LINE('',#3698,#921) ;
#654 = LINE('',#3701,#922) ;
#655 = LINE('',#3702,#923) ;
#656 = LINE('',#3705,#924) ;
#657 = LINE('',#3706,#925) ;
#658 = LINE('',#3708,#926) ;
#659 = LINE('',#3712,#927) ;
#660 = LINE('',#3714,#928) ;
#661 = LINE('',#3716,#929) ;
#662 = LINE('',#3717,#930) ;
#663 = LINE('',#3721,#931) ;
#664 = LINE('',#3723,#932) ;
#665 = LINE('',#3725,#933) ;
#666 = LINE('',#3726,#934) ;
#667 = LINE('',#3728,#935) ;
#668 = LINE('',#3729,#936) ;
#669 = LINE('',#3731,#937) ;
#670 = LINE('',#3733,#938) ;
#671 = VECTOR('',#2510,100.) ;
#672 = VECTOR('',#2511,100.) ;
#673 = VECTOR('',#2512,100.) ;
#674 = VECTOR('',#2513,100.) ;
#675 = VECTOR('',#2516,100.) ;
#676 = VECTOR('',#2517,100.) ;
#677 = VECTOR('',#2518,100.) ;
#678 = VECTOR('',#2521,100.) ;
#679 = VECTOR('',#2522,100.) ;
#680 = VECTOR('',#2523,100.) ;
#681 = VECTOR('',#2526,100.) ;
#682 = VECTOR('',#2527,100.) ;
#683 = VECTOR('',#2530,100.) ;
#684 = VECTOR('',#2531,100.) ;
#685 = VECTOR('',#2532,100.) ;
#686 = VECTOR('',#2533,100.) ;
#687 = VECTOR('',#2534,100.) ;
#688 = VECTOR('',#2535,100.) ;
#689 = VECTOR('',#2536,100.) ;
#690 = VECTOR('',#2537,100.) ;
#691 = VECTOR('',#2540,100.) ;
#692 = VECTOR('',#2541,100.) ;
#693 = VECTOR('',#2542,100.) ;
#694 = VECTOR('',#2543,100.) ;
#695 = VECTOR('',#2546,100.) ;
#696 = VECTOR('',#2547,100.) ;
#697 = VECTOR('',#2548,100.) ;
#698 = VECTOR('',#2549,100.) ;
#699 = VECTOR('',#2552,100.) ;
#700 = VECTOR('',#2553,100.) ;
#701 = VECTOR('',#2554,100.) ;
#702 = VECTOR('',#2555,100.) ;
#703 = VECTOR('',#2558,100.) ;
#704 = VECTOR('',#2559,100.) ;
#705 = VECTOR('',#2560,100.) ;
#706 = VECTOR('',#2561,100.) ;
#707 = VECTOR('',#2582,100.) ;
#708 = VECTOR('',#2583,100.) ;
#709 = VECTOR('',#2584,100.) ;
#710 = VECTOR('',#2585,100.) ;
#711 = VECTOR('',#2586,100.) ;
#712 = VECTOR('',#2587,100.) ;
#713 = VECTOR('',#2588,100.) ;
#714 = VECTOR('',#2589,100.) ;
#715 = VECTOR('',#2600,100.) ;
#716 = VECTOR('',#2601,100.) ;
#717 = VECTOR('',#2604,100.) ;
#718 = VECTOR('',#2607,100.) ;
#719 = VECTOR('',#2612,100.) ;
#720 = VECTOR('',#2613,100.) ;
#721 = VECTOR('',#2616,100.) ;
#722 = VECTOR('',#2619,100.) ;
#723 = VECTOR('',#2626,100.) ;
#724 = VECTOR('',#2627,100.) ;
#725 = VECTOR('',#2628,100.) ;
#726 = VECTOR('',#2629,100.) ;
#727 = VECTOR('',#2632,100.) ;
#728 = VECTOR('',#2633,100.) ;
#729 = VECTOR('',#2634,100.) ;
#730 = VECTOR('',#2637,100.) ;
#731 = VECTOR('',#2638,100.) ;
#732 = VECTOR('',#2639,100.) ;
#733 = VECTOR('',#2642,100.) ;
#734 = VECTOR('',#2643,100.) ;
#735 = VECTOR('',#2646,100.) ;
#736 = VECTOR('',#2647,100.) ;
#737 = VECTOR('',#2648,100.) ;
#738 = VECTOR('',#2649,100.) ;
#739 = VECTOR('',#2650,100.) ;
#740 = VECTOR('',#2651,100.) ;
#741 = VECTOR('',#2652,100.) ;
#742 = VECTOR('',#2653,100.) ;
#743 = VECTOR('',#2656,100.) ;
#744 = VECTOR('',#2657,100.) ;
#745 = VECTOR('',#2658,100.) ;
#746 = VECTOR('',#2659,100.) ;
#747 = VECTOR('',#2662,100.) ;
#748 = VECTOR('',#2663,100.) ;
#749 = VECTOR('',#2664,100.) ;
#750 = VECTOR('',#2665,100.) ;
#751 = VECTOR('',#2668,100.) ;
#752 = VECTOR('',#2669,100.) ;
#753 = VECTOR('',#2670,100.) ;
#754 = VECTOR('',#2671,100.) ;
#755 = VECTOR('',#2674,100.) ;
#756 = VECTOR('',#2675,100.) ;
#757 = VECTOR('',#2676,100.) ;
#758 = VECTOR('',#2677,100.) ;
#759 = VECTOR('',#2698,100.) ;
#760 = VECTOR('',#2699,100.) ;
#761 = VECTOR('',#2700,100.) ;
#762 = VECTOR('',#2701,100.) ;
#763 = VECTOR('',#2702,100.) ;
#764 = VECTOR('',#2703,100.) ;
#765 = VECTOR('',#2704,100.) ;
#766 = VECTOR('',#2705,100.) ;
#767 = VECTOR('',#2716,100.) ;
#768 = VECTOR('',#2717,100.) ;
#769 = VECTOR('',#2720,100.) ;
#770 = VECTOR('',#2723,100.) ;
#771 = VECTOR('',#2728,100.) ;
#772 = VECTOR('',#2729,100.) ;
#773 = VECTOR('',#2732,100.) ;
#774 = VECTOR('',#2735,100.) ;
#775 = VECTOR('',#2742,100.) ;
#776 = VECTOR('',#2743,100.) ;
#777 = VECTOR('',#2744,100.) ;
#778 = VECTOR('',#2745,100.) ;
#779 = VECTOR('',#2748,100.) ;
#780 = VECTOR('',#2749,100.) ;
#781 = VECTOR('',#2750,100.) ;
#782 = VECTOR('',#2753,100.) ;
#783 = VECTOR('',#2754,100.) ;
#784 = VECTOR('',#2755,100.) ;
#785 = VECTOR('',#2758,100.) ;
#786 = VECTOR('',#2759,100.) ;
#787 = VECTOR('',#2762,100.) ;
#788 = VECTOR('',#2763,100.) ;
#789 = VECTOR('',#2764,100.) ;
#790 = VECTOR('',#2765,100.) ;
#791 = VECTOR('',#2768,100.) ;
#792 = VECTOR('',#2769,100.) ;
#793 = VECTOR('',#2770,100.) ;
#794 = VECTOR('',#2771,100.) ;
#795 = VECTOR('',#2774,100.) ;
#796 = VECTOR('',#2775,100.) ;
#797 = VECTOR('',#2776,100.) ;
#798 = VECTOR('',#2777,100.) ;
#799 = VECTOR('',#2780,100.) ;
#800 = VECTOR('',#2781,100.) ;
#801 = VECTOR('',#2782,100.) ;
#802 = VECTOR('',#2783,100.) ;
#803 = VECTOR('',#2786,100.) ;
#804 = VECTOR('',#2787,100.) ;
#805 = VECTOR('',#2788,100.) ;
#806 = VECTOR('',#2789,100.) ;
#807 = VECTOR('',#2810,100.) ;
#808 = VECTOR('',#2811,100.) ;
#809 = VECTOR('',#2812,100.) ;
#810 = VECTOR('',#2813,100.) ;
#811 = VECTOR('',#2824,100.) ;
#812 = VECTOR('',#2825,100.) ;
#813 = VECTOR('',#2828,100.) ;
#814 = VECTOR('',#2831,100.) ;
#815 = VECTOR('',#2838,100.) ;
#816 = VECTOR('',#2839,100.) ;
#817 = VECTOR('',#2840,100.) ;
#818 = VECTOR('',#2841,100.) ;
#819 = VECTOR('',#2844,100.) ;
#820 = VECTOR('',#2845,100.) ;
#821 = VECTOR('',#2846,100.) ;
#822 = VECTOR('',#2849,100.) ;
#823 = VECTOR('',#2850,100.) ;
#824 = VECTOR('',#2851,100.) ;
#825 = VECTOR('',#2854,100.) ;
#826 = VECTOR('',#2855,100.) ;
#827 = VECTOR('',#2860,100.) ;
#828 = VECTOR('',#2861,100.) ;
#829 = VECTOR('',#2862,100.) ;
#830 = VECTOR('',#2863,100.) ;
#831 = VECTOR('',#2866,100.) ;
#832 = VECTOR('',#2867,100.) ;
#833 = VECTOR('',#2868,100.) ;
#834 = VECTOR('',#2869,100.) ;
#835 = VECTOR('',#2872,100.) ;
#836 = VECTOR('',#2873,100.) ;
#837 = VECTOR('',#2874,100.) ;
#838 = VECTOR('',#2875,100.) ;
#839 = VECTOR('',#2878,100.) ;
#840 = VECTOR('',#2879,100.) ;
#841 = VECTOR('',#2880,100.) ;
#842 = VECTOR('',#2881,100.) ;
#843 = VECTOR('',#2914,100.) ;
#844 = VECTOR('',#2915,100.) ;
#845 = VECTOR('',#2916,100.) ;
#846 = VECTOR('',#2917,100.) ;
#847 = VECTOR('',#2920,100.) ;
#848 = VECTOR('',#2921,100.) ;
#849 = VECTOR('',#2922,100.) ;
#850 = VECTOR('',#2925,100.) ;
#851 = VECTOR('',#2926,100.) ;
#852 = VECTOR('',#2927,100.) ;
#853 = VECTOR('',#2930,100.) ;
#854 = VECTOR('',#2931,100.) ;
#855 = VECTOR('',#2934,100.) ;
#856 = VECTOR('',#2935,100.) ;
#857 = VECTOR('',#2936,100.) ;
#858 = VECTOR('',#2937,100.) ;
#859 = VECTOR('',#2940,100.) ;
#860 = VECTOR('',#2941,100.) ;
#861 = VECTOR('',#2942,100.) ;
#862 = VECTOR('',#2943,100.) ;
#863 = VECTOR('',#2944,100.) ;
#864 = VECTOR('',#2945,100.) ;
#865 = VECTOR('',#2946,100.) ;
#866 = VECTOR('',#2947,100.) ;
#867 = VECTOR('',#2950,100.) ;
#868 = VECTOR('',#2951,100.) ;
#869 = VECTOR('',#2954,100.) ;
#870 = VECTOR('',#2957,100.) ;
#871 = VECTOR('',#2962,100.) ;
#872 = VECTOR('',#2963,100.) ;
#873 = VECTOR('',#2964,100.) ;
#874 = VECTOR('',#2967,100.) ;
#875 = VECTOR('',#2968,100.) ;
#876 = VECTOR('',#2971,100.) ;
#877 = VECTOR('',#2972,100.) ;
#878 = VECTOR('',#2975,100.) ;
#879 = VECTOR('',#2978,100.) ;
#880 = VECTOR('',#2979,100.) ;
#881 = VECTOR('',#2980,100.) ;
#882 = VECTOR('',#2981,100.) ;
#883 = VECTOR('',#2984,100.) ;
#884 = VECTOR('',#2985,100.) ;
#885 = VECTOR('',#2986,100.) ;
#886 = VECTOR('',#2987,100.) ;
#887 = VECTOR('',#2990,100.) ;
#888 = VECTOR('',#2991,100.) ;
#889 = VECTOR('',#2994,100.) ;
#890 = VECTOR('',#2997,100.) ;
#891 = VECTOR('',#3004,100.) ;
#892 = VECTOR('',#3005,100.) ;
#893 = VECTOR('',#3006,100.) ;
#894 = VECTOR('',#3007,100.) ;
#895 = VECTOR('',#3010,100.) ;
#896 = VECTOR('',#3011,100.) ;
#897 = VECTOR('',#3012,100.) ;
#898 = VECTOR('',#3015,100.) ;
#899 = VECTOR('',#3016,100.) ;
#900 = VECTOR('',#3017,100.) ;
#901 = VECTOR('',#3020,100.) ;
#902 = VECTOR('',#3021,100.) ;
#903 = VECTOR('',#3024,100.) ;
#904 = VECTOR('',#3025,100.) ;
#905 = VECTOR('',#3026,100.) ;
#906 = VECTOR('',#3027,100.) ;
#907 = VECTOR('',#3030,100.) ;
#908 = VECTOR('',#3031,100.) ;
#909 = VECTOR('',#3032,100.) ;
#910 = VECTOR('',#3033,100.) ;
#911 = VECTOR('',#3034,100.) ;
#912 = VECTOR('',#3035,100.) ;
#913 = VECTOR('',#3036,100.) ;
#914 = VECTOR('',#3037,100.) ;
#915 = VECTOR('',#3040,100.) ;
#916 = VECTOR('',#3041,100.) ;
#917 = VECTOR('',#3044,100.) ;
#918 = VECTOR('',#3047,100.) ;
#919 = VECTOR('',#3052,100.) ;
#920 = VECTOR('',#3053,100.) ;
#921 = VECTOR('',#3054,100.) ;
#922 = VECTOR('',#3057,100.) ;
#923 = VECTOR('',#3058,100.) ;
#924 = VECTOR('',#3061,100.) ;
#925 = VECTOR('',#3062,100.) ;
#926 = VECTOR('',#3065,100.) ;
#927 = VECTOR('',#3068,100.) ;
#928 = VECTOR('',#3069,100.) ;
#929 = VECTOR('',#3070,100.) ;
#930 = VECTOR('',#3071,100.) ;
#931 = VECTOR('',#3074,100.) ;
#932 = VECTOR('',#3075,100.) ;
#933 = VECTOR('',#3076,100.) ;
#934 = VECTOR('',#3077,100.) ;
#935 = VECTOR('',#3080,100.) ;
#936 = VECTOR('',#3081,100.) ;
#937 = VECTOR('',#3084,100.) ;
#938 = VECTOR('',#3087,100.) ;
#939 = VERTEX_POINT('',#3111) ;
#940 = VERTEX_POINT('',#3112) ;
#941 = VERTEX_POINT('',#3114) ;
#942 = VERTEX_POINT('',#3116) ;
#943 = VERTEX_POINT('',#3120) ;
#944 = VERTEX_POINT('',#3122) ;
#945 = VERTEX_POINT('',#3126) ;
#946 = VERTEX_POINT('',#3128) ;
#947 = VERTEX_POINT('',#3135) ;
#948 = VERTEX_POINT('',#3136) ;
#949 = VERTEX_POINT('',#3138) ;
#950 = VERTEX_POINT('',#3140) ;
#951 = VERTEX_POINT('',#3143) ;
#952 = VERTEX_POINT('',#3144) ;
#953 = VERTEX_POINT('',#3146) ;
#954 = VERTEX_POINT('',#3148) ;
#955 = VERTEX_POINT('',#3152) ;
#956 = VERTEX_POINT('',#3153) ;
#957 = VERTEX_POINT('',#3155) ;
#958 = VERTEX_POINT('',#3157) ;
#959 = VERTEX_POINT('',#3161) ;
#960 = VERTEX_POINT('',#3162) ;
#961 = VERTEX_POINT('',#3164) ;
#962 = VERTEX_POINT('',#3166) ;
#963 = VERTEX_POINT('',#3170) ;
#964 = VERTEX_POINT('',#3171) ;
#965 = VERTEX_POINT('',#3173) ;
#966 = VERTEX_POINT('',#3175) ;
#967 = VERTEX_POINT('',#3179) ;
#968 = VERTEX_POINT('',#3180) ;
#969 = VERTEX_POINT('',#3182) ;
#970 = VERTEX_POINT('',#3184) ;
#971 = VERTEX_POINT('',#3197) ;
#972 = VERTEX_POINT('',#3198) ;
#973 = VERTEX_POINT('',#3200) ;
#974 = VERTEX_POINT('',#3202) ;
#975 = VERTEX_POINT('',#3205) ;
#976 = VERTEX_POINT('',#3206) ;
#977 = VERTEX_POINT('',#3208) ;
#978 = VERTEX_POINT('',#3210) ;
#979 = VERTEX_POINT('',#3235) ;
#980 = VERTEX_POINT('',#3236) ;
#981 = VERTEX_POINT('',#3238) ;
#982 = VERTEX_POINT('',#3240) ;
#983 = VERTEX_POINT('',#3244) ;
#984 = VERTEX_POINT('',#3246) ;
#985 = VERTEX_POINT('',#3250) ;
#986 = VERTEX_POINT('',#3252) ;
#987 = VERTEX_POINT('',#3259) ;
#988 = VERTEX_POINT('',#3260) ;
#989 = VERTEX_POINT('',#3262) ;
#990 = VERTEX_POINT('',#3264) ;
#991 = VERTEX_POINT('',#3267) ;
#992 = VERTEX_POINT('',#3268) ;
#993 = VERTEX_POINT('',#3270) ;
#994 = VERTEX_POINT('',#3272) ;
#995 = VERTEX_POINT('',#3276) ;
#996 = VERTEX_POINT('',#3277) ;
#997 = VERTEX_POINT('',#3279) ;
#998 = VERTEX_POINT('',#3281) ;
#999 = VERTEX_POINT('',#3285) ;
#1000 = VERTEX_POINT('',#3286) ;
#1001 = VERTEX_POINT('',#3288) ;
#1002 = VERTEX_POINT('',#3290) ;
#1003 = VERTEX_POINT('',#3294) ;
#1004 = VERTEX_POINT('',#3295) ;
#1005 = VERTEX_POINT('',#3297) ;
#1006 = VERTEX_POINT('',#3299) ;
#1007 = VERTEX_POINT('',#3303) ;
#1008 = VERTEX_POINT('',#3304) ;
#1009 = VERTEX_POINT('',#3306) ;
#1010 = VERTEX_POINT('',#3308) ;
#1011 = VERTEX_POINT('',#3321) ;
#1012 = VERTEX_POINT('',#3322) ;
#1013 = VERTEX_POINT('',#3324) ;
#1014 = VERTEX_POINT('',#3326) ;
#1015 = VERTEX_POINT('',#3329) ;
#1016 = VERTEX_POINT('',#3330) ;
#1017 = VERTEX_POINT('',#3332) ;
#1018 = VERTEX_POINT('',#3334) ;
#1019 = VERTEX_POINT('',#3359) ;
#1020 = VERTEX_POINT('',#3360) ;
#1021 = VERTEX_POINT('',#3362) ;
#1022 = VERTEX_POINT('',#3364) ;
#1023 = VERTEX_POINT('',#3368) ;
#1024 = VERTEX_POINT('',#3370) ;
#1025 = VERTEX_POINT('',#3374) ;
#1026 = VERTEX_POINT('',#3376) ;
#1027 = VERTEX_POINT('',#3383) ;
#1028 = VERTEX_POINT('',#3384) ;
#1029 = VERTEX_POINT('',#3386) ;
#1030 = VERTEX_POINT('',#3388) ;
#1031 = VERTEX_POINT('',#3392) ;
#1032 = VERTEX_POINT('',#3393) ;
#1033 = VERTEX_POINT('',#3395) ;
#1034 = VERTEX_POINT('',#3397) ;
#1035 = VERTEX_POINT('',#3401) ;
#1036 = VERTEX_POINT('',#3402) ;
#1037 = VERTEX_POINT('',#3404) ;
#1038 = VERTEX_POINT('',#3406) ;
#1039 = VERTEX_POINT('',#3410) ;
#1040 = VERTEX_POINT('',#3411) ;
#1041 = VERTEX_POINT('',#3413) ;
#1042 = VERTEX_POINT('',#3415) ;
#1043 = VERTEX_POINT('',#3419) ;
#1044 = VERTEX_POINT('',#3420) ;
#1045 = VERTEX_POINT('',#3422) ;
#1046 = VERTEX_POINT('',#3424) ;
#1047 = VERTEX_POINT('',#3437) ;
#1048 = VERTEX_POINT('',#3438) ;
#1049 = VERTEX_POINT('',#3440) ;
#1050 = VERTEX_POINT('',#3442) ;
#1051 = VERTEX_POINT('',#3459) ;
#1052 = VERTEX_POINT('',#3460) ;
#1053 = VERTEX_POINT('',#3462) ;
#1054 = VERTEX_POINT('',#3464) ;
#1055 = VERTEX_POINT('',#3468) ;
#1056 = VERTEX_POINT('',#3470) ;
#1057 = VERTEX_POINT('',#3474) ;
#1058 = VERTEX_POINT('',#3476) ;
#1059 = VERTEX_POINT('',#3484) ;
#1060 = VERTEX_POINT('',#3485) ;
#1061 = VERTEX_POINT('',#3487) ;
#1062 = VERTEX_POINT('',#3489) ;
#1063 = VERTEX_POINT('',#3493) ;
#1064 = VERTEX_POINT('',#3494) ;
#1065 = VERTEX_POINT('',#3496) ;
#1066 = VERTEX_POINT('',#3498) ;
#1067 = VERTEX_POINT('',#3502) ;
#1068 = VERTEX_POINT('',#3503) ;
#1069 = VERTEX_POINT('',#3505) ;
#1070 = VERTEX_POINT('',#3507) ;
#1071 = VERTEX_POINT('',#3511) ;
#1072 = VERTEX_POINT('',#3512) ;
#1073 = VERTEX_POINT('',#3514) ;
#1074 = VERTEX_POINT('',#3516) ;
#1075 = VERTEX_POINT('',#3535) ;
#1076 = VERTEX_POINT('',#3536) ;
#1077 = VERTEX_POINT('',#3538) ;
#1078 = VERTEX_POINT('',#3540) ;
#1079 = VERTEX_POINT('',#3544) ;
#1080 = VERTEX_POINT('',#3546) ;
#1081 = VERTEX_POINT('',#3550) ;
#1082 = VERTEX_POINT('',#3552) ;
#1083 = VERTEX_POINT('',#3559) ;
#1084 = VERTEX_POINT('',#3560) ;
#1085 = VERTEX_POINT('',#3562) ;
#1086 = VERTEX_POINT('',#3564) ;
#1087 = VERTEX_POINT('',#3568) ;
#1088 = VERTEX_POINT('',#3569) ;
#1089 = VERTEX_POINT('',#3571) ;
#1090 = VERTEX_POINT('',#3573) ;
#1091 = VERTEX_POINT('',#3576) ;
#1092 = VERTEX_POINT('',#3577) ;
#1093 = VERTEX_POINT('',#3579) ;
#1094 = VERTEX_POINT('',#3581) ;
#1095 = VERTEX_POINT('',#3593) ;
#1096 = VERTEX_POINT('',#3595) ;
#1097 = VERTEX_POINT('',#3599) ;
#1098 = VERTEX_POINT('',#3603) ;
#1099 = VERTEX_POINT('',#3609) ;
#1100 = VERTEX_POINT('',#3610) ;
#1101 = VERTEX_POINT('',#3612) ;
#1102 = VERTEX_POINT('',#3614) ;
#1103 = VERTEX_POINT('',#3618) ;
#1104 = VERTEX_POINT('',#3619) ;
#1105 = VERTEX_POINT('',#3621) ;
#1106 = VERTEX_POINT('',#3623) ;
#1107 = VERTEX_POINT('',#3636) ;
#1108 = VERTEX_POINT('',#3637) ;
#1109 = VERTEX_POINT('',#3639) ;
#1110 = VERTEX_POINT('',#3641) ;
#1111 = VERTEX_POINT('',#3645) ;
#1112 = VERTEX_POINT('',#3647) ;
#1113 = VERTEX_POINT('',#3651) ;
#1114 = VERTEX_POINT('',#3653) ;
#1115 = VERTEX_POINT('',#3660) ;
#1116 = VERTEX_POINT('',#3661) ;
#1117 = VERTEX_POINT('',#3663) ;
#1118 = VERTEX_POINT('',#3665) ;
#1119 = VERTEX_POINT('',#3669) ;
#1120 = VERTEX_POINT('',#3670) ;
#1121 = VERTEX_POINT('',#3672) ;
#1122 = VERTEX_POINT('',#3674) ;
#1123 = VERTEX_POINT('',#3677) ;
#1124 = VERTEX_POINT('',#3678) ;
#1125 = VERTEX_POINT('',#3680) ;
#1126 = VERTEX_POINT('',#3682) ;
#1127 = VERTEX_POINT('',#3694) ;
#1128 = VERTEX_POINT('',#3696) ;
#1129 = VERTEX_POINT('',#3700) ;
#1130 = VERTEX_POINT('',#3704) ;
#1131 = VERTEX_POINT('',#3710) ;
#1132 = VERTEX_POINT('',#3711) ;
#1133 = VERTEX_POINT('',#3713) ;
#1134 = VERTEX_POINT('',#3715) ;
#1135 = VERTEX_POINT('',#3719) ;
#1136 = VERTEX_POINT('',#3720) ;
#1137 = VERTEX_POINT('',#3722) ;
#1138 = VERTEX_POINT('',#3724) ;
#1139 = EDGE_CURVE('',#939,#940,#403,.T.) ;
#1140 = EDGE_CURVE('',#941,#939,#404,.T.) ;
#1141 = EDGE_CURVE('',#941,#942,#405,.T.) ;
#1142 = EDGE_CURVE('',#942,#940,#406,.T.) ;
#1143 = EDGE_CURVE('',#939,#943,#407,.T.) ;
#1144 = EDGE_CURVE('',#944,#943,#408,.T.) ;
#1145 = EDGE_CURVE('',#941,#944,#409,.T.) ;
#1146 = EDGE_CURVE('',#943,#945,#410,.T.) ;
#1147 = EDGE_CURVE('',#946,#945,#411,.T.) ;
#1148 = EDGE_CURVE('',#944,#946,#412,.T.) ;
#1149 = EDGE_CURVE('',#940,#945,#413,.T.) ;
#1150 = EDGE_CURVE('',#942,#946,#414,.T.) ;
#1151 = EDGE_CURVE('',#947,#948,#415,.T.) ;
#1152 = EDGE_CURVE('',#948,#949,#416,.T.) ;
#1153 = EDGE_CURVE('',#949,#950,#417,.T.) ;
#1154 = EDGE_CURVE('',#950,#947,#418,.T.) ;
#1155 = EDGE_CURVE('',#951,#952,#419,.T.) ;
#1156 = EDGE_CURVE('',#952,#953,#420,.T.) ;
#1157 = EDGE_CURVE('',#953,#954,#421,.T.) ;
#1158 = EDGE_CURVE('',#954,#951,#422,.T.) ;
#1159 = EDGE_CURVE('',#955,#956,#423,.T.) ;
#1160 = EDGE_CURVE('',#955,#957,#424,.T.) ;
#1161 = EDGE_CURVE('',#957,#958,#425,.T.) ;
#1162 = EDGE_CURVE('',#958,#956,#426,.T.) ;
#1163 = EDGE_CURVE('',#959,#960,#427,.T.) ;
#1164 = EDGE_CURVE('',#960,#961,#428,.T.) ;
#1165 = EDGE_CURVE('',#962,#961,#429,.T.) ;
#1166 = EDGE_CURVE('',#962,#959,#430,.T.) ;
#1167 = EDGE_CURVE('',#963,#964,#431,.T.) ;
#1168 = EDGE_CURVE('',#963,#965,#432,.T.) ;
#1169 = EDGE_CURVE('',#965,#966,#433,.T.) ;
#1170 = EDGE_CURVE('',#966,#964,#434,.T.) ;
#1171 = EDGE_CURVE('',#967,#968,#435,.T.) ;
#1172 = EDGE_CURVE('',#967,#969,#436,.T.) ;
#1173 = EDGE_CURVE('',#969,#970,#437,.T.) ;
#1174 = EDGE_CURVE('',#970,#968,#438,.T.) ;
#1175 = EDGE_CURVE('',#969,#955,#87,.T.) ;
#1176 = EDGE_CURVE('',#956,#962,#88,.T.) ;
#1177 = EDGE_CURVE('',#961,#966,#89,.T.) ;
#1178 = EDGE_CURVE('',#965,#970,#90,.T.) ;
#1179 = EDGE_CURVE('',#957,#967,#91,.T.) ;
#1180 = EDGE_CURVE('',#968,#963,#92,.T.) ;
#1181 = EDGE_CURVE('',#964,#960,#93,.T.) ;
#1182 = EDGE_CURVE('',#959,#958,#94,.T.) ;
#1183 = EDGE_CURVE('',#971,#972,#439,.T.) ;
#1184 = EDGE_CURVE('',#973,#971,#440,.T.) ;
#1185 = EDGE_CURVE('',#974,#973,#441,.T.) ;
#1186 = EDGE_CURVE('',#972,#974,#442,.T.) ;
#1187 = EDGE_CURVE('',#975,#976,#443,.T.) ;
#1188 = EDGE_CURVE('',#977,#975,#444,.T.) ;
#1189 = EDGE_CURVE('',#978,#977,#445,.T.) ;
#1190 = EDGE_CURVE('',#976,#978,#446,.T.) ;
#1191 = EDGE_CURVE('',#952,#975,#447,.T.) ;
#1192 = EDGE_CURVE('',#953,#976,#448,.T.) ;
#1193 = EDGE_CURVE('',#951,#977,#449,.T.) ;
#1194 = EDGE_CURVE('',#954,#978,#450,.T.) ;
#1195 = EDGE_CURVE('',#948,#971,#451,.T.) ;
#1196 = EDGE_CURVE('',#949,#972,#452,.T.) ;
#1197 = EDGE_CURVE('',#947,#973,#453,.T.) ;
#1198 = EDGE_CURVE('',#950,#974,#454,.T.) ;
#1199 = EDGE_CURVE('',#979,#980,#455,.T.) ;
#1200 = EDGE_CURVE('',#981,#979,#456,.T.) ;
#1201 = EDGE_CURVE('',#981,#982,#457,.T.) ;
#1202 = EDGE_CURVE('',#982,#980,#458,.T.) ;
#1203 = EDGE_CURVE('',#979,#983,#459,.T.) ;
#1204 = EDGE_CURVE('',#984,#983,#460,.T.) ;
#1205 = EDGE_CURVE('',#981,#984,#461,.T.) ;
#1206 = EDGE_CURVE('',#983,#985,#462,.T.) ;
#1207 = EDGE_CURVE('',#986,#985,#463,.T.) ;
#1208 = EDGE_CURVE('',#984,#986,#464,.T.) ;
#1209 = EDGE_CURVE('',#980,#985,#465,.T.) ;
#1210 = EDGE_CURVE('',#982,#986,#466,.T.) ;
#1211 = EDGE_CURVE('',#987,#988,#467,.T.) ;
#1212 = EDGE_CURVE('',#988,#989,#468,.T.) ;
#1213 = EDGE_CURVE('',#989,#990,#469,.T.) ;
#1214 = EDGE_CURVE('',#990,#987,#470,.T.) ;
#1215 = EDGE_CURVE('',#991,#992,#471,.T.) ;
#1216 = EDGE_CURVE('',#992,#993,#472,.T.) ;
#1217 = EDGE_CURVE('',#993,#994,#473,.T.) ;
#1218 = EDGE_CURVE('',#994,#991,#474,.T.) ;
#1219 = EDGE_CURVE('',#995,#996,#475,.T.) ;
#1220 = EDGE_CURVE('',#995,#997,#476,.T.) ;
#1221 = EDGE_CURVE('',#997,#998,#477,.T.) ;
#1222 = EDGE_CURVE('',#998,#996,#478,.T.) ;
#1223 = EDGE_CURVE('',#999,#1000,#479,.T.) ;
#1224 = EDGE_CURVE('',#1000,#1001,#480,.T.) ;
#1225 = EDGE_CURVE('',#1002,#1001,#481,.T.) ;
#1226 = EDGE_CURVE('',#1002,#999,#482,.T.) ;
#1227 = EDGE_CURVE('',#1003,#1004,#483,.T.) ;
#1228 = EDGE_CURVE('',#1003,#1005,#484,.T.) ;
#1229 = EDGE_CURVE('',#1005,#1006,#485,.T.) ;
#1230 = EDGE_CURVE('',#1006,#1004,#486,.T.) ;
#1231 = EDGE_CURVE('',#1007,#1008,#487,.T.) ;
#1232 = EDGE_CURVE('',#1007,#1009,#488,.T.) ;
#1233 = EDGE_CURVE('',#1009,#1010,#489,.T.) ;
#1234 = EDGE_CURVE('',#1010,#1008,#490,.T.) ;
#1235 = EDGE_CURVE('',#1009,#995,#95,.T.) ;
#1236 = EDGE_CURVE('',#996,#1002,#96,.T.) ;
#1237 = EDGE_CURVE('',#1001,#1006,#97,.T.) ;
#1238 = EDGE_CURVE('',#1005,#1010,#98,.T.) ;
#1239 = EDGE_CURVE('',#997,#1007,#99,.T.) ;
#1240 = EDGE_CURVE('',#1008,#1003,#100,.T.) ;
#1241 = EDGE_CURVE('',#1004,#1000,#101,.T.) ;
#1242 = EDGE_CURVE('',#999,#998,#102,.T.) ;
#1243 = EDGE_CURVE('',#1011,#1012,#491,.T.) ;
#1244 = EDGE_CURVE('',#1013,#1011,#492,.T.) ;
#1245 = EDGE_CURVE('',#1014,#1013,#493,.T.) ;
#1246 = EDGE_CURVE('',#1012,#1014,#494,.T.) ;
#1247 = EDGE_CURVE('',#1015,#1016,#495,.T.) ;
#1248 = EDGE_CURVE('',#1017,#1015,#496,.T.) ;
#1249 = EDGE_CURVE('',#1018,#1017,#497,.T.) ;
#1250 = EDGE_CURVE('',#1016,#1018,#498,.T.) ;
#1251 = EDGE_CURVE('',#992,#1015,#499,.T.) ;
#1252 = EDGE_CURVE('',#993,#1016,#500,.T.) ;
#1253 = EDGE_CURVE('',#991,#1017,#501,.T.) ;
#1254 = EDGE_CURVE('',#994,#1018,#502,.T.) ;
#1255 = EDGE_CURVE('',#988,#1011,#503,.T.) ;
#1256 = EDGE_CURVE('',#989,#1012,#504,.T.) ;
#1257 = EDGE_CURVE('',#987,#1013,#505,.T.) ;
#1258 = EDGE_CURVE('',#990,#1014,#506,.T.) ;
#1259 = EDGE_CURVE('',#1019,#1020,#507,.T.) ;
#1260 = EDGE_CURVE('',#1021,#1019,#508,.T.) ;
#1261 = EDGE_CURVE('',#1021,#1022,#509,.T.) ;
#1262 = EDGE_CURVE('',#1022,#1020,#510,.T.) ;
#1263 = EDGE_CURVE('',#1019,#1023,#511,.T.) ;
#1264 = EDGE_CURVE('',#1024,#1023,#512,.T.) ;
#1265 = EDGE_CURVE('',#1021,#1024,#513,.T.) ;
#1266 = EDGE_CURVE('',#1023,#1025,#514,.T.) ;
#1267 = EDGE_CURVE('',#1026,#1025,#515,.T.) ;
#1268 = EDGE_CURVE('',#1024,#1026,#516,.T.) ;
#1269 = EDGE_CURVE('',#1020,#1025,#517,.T.) ;
#1270 = EDGE_CURVE('',#1022,#1026,#518,.T.) ;
#1271 = EDGE_CURVE('',#1027,#1028,#519,.T.) ;
#1272 = EDGE_CURVE('',#1028,#1029,#520,.T.) ;
#1273 = EDGE_CURVE('',#1029,#1030,#521,.T.) ;
#1274 = EDGE_CURVE('',#1030,#1027,#522,.T.) ;
#1275 = EDGE_CURVE('',#1031,#1032,#523,.T.) ;
#1276 = EDGE_CURVE('',#1031,#1033,#524,.T.) ;
#1277 = EDGE_CURVE('',#1033,#1034,#525,.T.) ;
#1278 = EDGE_CURVE('',#1034,#1032,#526,.T.) ;
#1279 = EDGE_CURVE('',#1035,#1036,#527,.T.) ;
#1280 = EDGE_CURVE('',#1036,#1037,#528,.T.) ;
#1281 = EDGE_CURVE('',#1038,#1037,#529,.T.) ;
#1282 = EDGE_CURVE('',#1038,#1035,#530,.T.) ;
#1283 = EDGE_CURVE('',#1039,#1040,#531,.T.) ;
#1284 = EDGE_CURVE('',#1039,#1041,#532,.T.) ;
#1285 = EDGE_CURVE('',#1041,#1042,#533,.T.) ;
#1286 = EDGE_CURVE('',#1042,#1040,#534,.T.) ;
#1287 = EDGE_CURVE('',#1043,#1044,#535,.T.) ;
#1288 = EDGE_CURVE('',#1043,#1045,#536,.T.) ;
#1289 = EDGE_CURVE('',#1045,#1046,#537,.T.) ;
#1290 = EDGE_CURVE('',#1046,#1044,#538,.T.) ;
#1291 = EDGE_CURVE('',#1045,#1031,#103,.T.) ;
#1292 = EDGE_CURVE('',#1032,#1038,#104,.T.) ;
#1293 = EDGE_CURVE('',#1037,#1042,#105,.T.) ;
#1294 = EDGE_CURVE('',#1041,#1046,#106,.T.) ;
#1295 = EDGE_CURVE('',#1033,#1043,#107,.T.) ;
#1296 = EDGE_CURVE('',#1044,#1039,#108,.T.) ;
#1297 = EDGE_CURVE('',#1040,#1036,#109,.T.) ;
#1298 = EDGE_CURVE('',#1035,#1034,#110,.T.) ;
#1299 = EDGE_CURVE('',#1047,#1048,#539,.T.) ;
#1300 = EDGE_CURVE('',#1049,#1047,#540,.T.) ;
#1301 = EDGE_CURVE('',#1050,#1049,#541,.T.) ;
#1302 = EDGE_CURVE('',#1048,#1050,#542,.T.) ;
#1303 = EDGE_CURVE('',#1028,#1047,#543,.T.) ;
#1304 = EDGE_CURVE('',#1029,#1048,#544,.T.) ;
#1305 = EDGE_CURVE('',#1027,#1049,#545,.T.) ;
#1306 = EDGE_CURVE('',#1030,#1050,#546,.T.) ;
#1307 = EDGE_CURVE('',#1051,#1052,#547,.T.) ;
#1308 = EDGE_CURVE('',#1053,#1051,#548,.T.) ;
#1309 = EDGE_CURVE('',#1053,#1054,#549,.T.) ;
#1310 = EDGE_CURVE('',#1054,#1052,#550,.T.) ;
#1311 = EDGE_CURVE('',#1051,#1055,#551,.T.) ;
#1312 = EDGE_CURVE('',#1056,#1055,#552,.T.) ;
#1313 = EDGE_CURVE('',#1053,#1056,#553,.T.) ;
#1314 = EDGE_CURVE('',#1055,#1057,#554,.T.) ;
#1315 = EDGE_CURVE('',#1058,#1057,#555,.T.) ;
#1316 = EDGE_CURVE('',#1056,#1058,#556,.T.) ;
#1317 = EDGE_CURVE('',#1052,#1057,#557,.T.) ;
#1318 = EDGE_CURVE('',#1054,#1058,#558,.T.) ;
#1319 = EDGE_CURVE('',#1059,#1060,#559,.T.) ;
#1320 = EDGE_CURVE('',#1059,#1061,#560,.T.) ;
#1321 = EDGE_CURVE('',#1061,#1062,#561,.T.) ;
#1322 = EDGE_CURVE('',#1062,#1060,#562,.T.) ;
#1323 = EDGE_CURVE('',#1063,#1064,#563,.T.) ;
#1324 = EDGE_CURVE('',#1064,#1065,#564,.T.) ;
#1325 = EDGE_CURVE('',#1066,#1065,#565,.T.) ;
#1326 = EDGE_CURVE('',#1066,#1063,#566,.T.) ;
#1327 = EDGE_CURVE('',#1067,#1068,#567,.T.) ;
#1328 = EDGE_CURVE('',#1067,#1069,#568,.T.) ;
#1329 = EDGE_CURVE('',#1069,#1070,#569,.T.) ;
#1330 = EDGE_CURVE('',#1070,#1068,#570,.T.) ;
#1331 = EDGE_CURVE('',#1071,#1072,#571,.T.) ;
#1332 = EDGE_CURVE('',#1071,#1073,#572,.T.) ;
#1333 = EDGE_CURVE('',#1073,#1074,#573,.T.) ;
#1334 = EDGE_CURVE('',#1074,#1072,#574,.T.) ;
#1335 = EDGE_CURVE('',#1073,#1059,#111,.T.) ;
#1336 = EDGE_CURVE('',#1060,#1066,#112,.T.) ;
#1337 = EDGE_CURVE('',#1065,#1070,#113,.T.) ;
#1338 = EDGE_CURVE('',#1069,#1074,#114,.T.) ;
#1339 = EDGE_CURVE('',#1061,#1071,#115,.T.) ;
#1340 = EDGE_CURVE('',#1072,#1067,#116,.T.) ;
#1341 = EDGE_CURVE('',#1068,#1064,#117,.T.) ;
#1342 = EDGE_CURVE('',#1063,#1062,#118,.T.) ;
#1343 = EDGE_CURVE('',#1075,#1076,#575,.T.) ;
#1344 = EDGE_CURVE('',#1075,#1077,#576,.T.) ;
#1345 = EDGE_CURVE('',#1078,#1077,#577,.T.) ;
#1346 = EDGE_CURVE('',#1076,#1078,#578,.T.) ;
#1347 = EDGE_CURVE('',#1076,#1079,#579,.T.) ;
#1348 = EDGE_CURVE('',#1080,#1078,#580,.T.) ;
#1349 = EDGE_CURVE('',#1079,#1080,#581,.T.) ;
#1350 = EDGE_CURVE('',#1079,#1081,#582,.T.) ;
#1351 = EDGE_CURVE('',#1082,#1080,#583,.T.) ;
#1352 = EDGE_CURVE('',#1081,#1082,#584,.T.) ;
#1353 = EDGE_CURVE('',#1081,#1075,#585,.T.) ;
#1354 = EDGE_CURVE('',#1077,#1082,#586,.T.) ;
#1355 = EDGE_CURVE('',#1083,#1084,#587,.T.) ;
#1356 = EDGE_CURVE('',#1084,#1085,#588,.T.) ;
#1357 = EDGE_CURVE('',#1085,#1086,#589,.T.) ;
#1358 = EDGE_CURVE('',#1086,#1083,#590,.T.) ;
#1359 = EDGE_CURVE('',#1087,#1088,#591,.T.) ;
#1360 = EDGE_CURVE('',#1089,#1087,#592,.T.) ;
#1361 = EDGE_CURVE('',#1090,#1089,#593,.T.) ;
#1362 = EDGE_CURVE('',#1088,#1090,#594,.T.) ;
#1363 = EDGE_CURVE('',#1091,#1092,#595,.T.) ;
#1364 = EDGE_CURVE('',#1092,#1093,#596,.T.) ;
#1365 = EDGE_CURVE('',#1093,#1094,#597,.T.) ;
#1366 = EDGE_CURVE('',#1094,#1091,#598,.T.) ;
#1367 = EDGE_CURVE('',#1084,#1088,#599,.T.) ;
#1368 = EDGE_CURVE('',#1083,#1087,#600,.T.) ;
#1369 = EDGE_CURVE('',#1085,#1090,#601,.T.) ;
#1370 = EDGE_CURVE('',#1086,#1089,#602,.T.) ;
#1371 = EDGE_CURVE('',#1095,#1092,#603,.T.) ;
#1372 = EDGE_CURVE('',#1096,#1091,#604,.T.) ;
#1373 = EDGE_CURVE('',#1096,#1095,#605,.T.) ;
#1374 = EDGE_CURVE('',#1097,#1093,#606,.T.) ;
#1375 = EDGE_CURVE('',#1095,#1097,#607,.T.) ;
#1376 = EDGE_CURVE('',#1098,#1094,#608,.T.) ;
#1377 = EDGE_CURVE('',#1097,#1098,#609,.T.) ;
#1378 = EDGE_CURVE('',#1098,#1096,#610,.T.) ;
#1379 = EDGE_CURVE('',#1099,#1100,#611,.T.) ;
#1380 = EDGE_CURVE('',#1100,#1101,#612,.T.) ;
#1381 = EDGE_CURVE('',#1101,#1102,#613,.T.) ;
#1382 = EDGE_CURVE('',#1102,#1099,#614,.T.) ;
#1383 = EDGE_CURVE('',#1103,#1104,#615,.T.) ;
#1384 = EDGE_CURVE('',#1105,#1103,#616,.T.) ;
#1385 = EDGE_CURVE('',#1106,#1105,#617,.T.) ;
#1386 = EDGE_CURVE('',#1104,#1106,#618,.T.) ;
#1387 = EDGE_CURVE('',#1103,#1099,#619,.T.) ;
#1388 = EDGE_CURVE('',#1104,#1100,#620,.T.) ;
#1389 = EDGE_CURVE('',#1105,#1102,#621,.T.) ;
#1390 = EDGE_CURVE('',#1106,#1101,#622,.T.) ;
#1391 = EDGE_CURVE('',#1107,#1108,#623,.T.) ;
#1392 = EDGE_CURVE('',#1107,#1109,#624,.T.) ;
#1393 = EDGE_CURVE('',#1110,#1109,#625,.T.) ;
#1394 = EDGE_CURVE('',#1108,#1110,#626,.T.) ;
#1395 = EDGE_CURVE('',#1108,#1111,#627,.T.) ;
#1396 = EDGE_CURVE('',#1112,#1110,#628,.T.) ;
#1397 = EDGE_CURVE('',#1111,#1112,#629,.T.) ;
#1398 = EDGE_CURVE('',#1111,#1113,#630,.T.) ;
#1399 = EDGE_CURVE('',#1114,#1112,#631,.T.) ;
#1400 = EDGE_CURVE('',#1113,#1114,#632,.T.) ;
#1401 = EDGE_CURVE('',#1113,#1107,#633,.T.) ;
#1402 = EDGE_CURVE('',#1109,#1114,#634,.T.) ;
#1403 = EDGE_CURVE('',#1115,#1116,#635,.T.) ;
#1404 = EDGE_CURVE('',#1116,#1117,#636,.T.) ;
#1405 = EDGE_CURVE('',#1117,#1118,#637,.T.) ;
#1406 = EDGE_CURVE('',#1118,#1115,#638,.T.) ;
#1407 = EDGE_CURVE('',#1119,#1120,#639,.T.) ;
#1408 = EDGE_CURVE('',#1121,#1119,#640,.T.) ;
#1409 = EDGE_CURVE('',#1122,#1121,#641,.T.) ;
#1410 = EDGE_CURVE('',#1120,#1122,#642,.T.) ;
#1411 = EDGE_CURVE('',#1123,#1124,#643,.T.) ;
#1412 = EDGE_CURVE('',#1124,#1125,#644,.T.) ;
#1413 = EDGE_CURVE('',#1125,#1126,#645,.T.) ;
#1414 = EDGE_CURVE('',#1126,#1123,#646,.T.) ;
#1415 = EDGE_CURVE('',#1116,#1120,#647,.T.) ;
#1416 = EDGE_CURVE('',#1115,#1119,#648,.T.) ;
#1417 = EDGE_CURVE('',#1117,#1122,#649,.T.) ;
#1418 = EDGE_CURVE('',#1118,#1121,#650,.T.) ;
#1419 = EDGE_CURVE('',#1127,#1124,#651,.T.) ;
#1420 = EDGE_CURVE('',#1128,#1123,#652,.T.) ;
#1421 = EDGE_CURVE('',#1128,#1127,#653,.T.) ;
#1422 = EDGE_CURVE('',#1129,#1125,#654,.T.) ;
#1423 = EDGE_CURVE('',#1127,#1129,#655,.T.) ;
#1424 = EDGE_CURVE('',#1130,#1126,#656,.T.) ;
#1425 = EDGE_CURVE('',#1129,#1130,#657,.T.) ;
#1426 = EDGE_CURVE('',#1130,#1128,#658,.T.) ;
#1427 = EDGE_CURVE('',#1131,#1132,#659,.T.) ;
#1428 = EDGE_CURVE('',#1132,#1133,#660,.T.) ;
#1429 = EDGE_CURVE('',#1133,#1134,#661,.T.) ;
#1430 = EDGE_CURVE('',#1134,#1131,#662,.T.) ;
#1431 = EDGE_CURVE('',#1135,#1136,#663,.T.) ;
#1432 = EDGE_CURVE('',#1137,#1135,#664,.T.) ;
#1433 = EDGE_CURVE('',#1138,#1137,#665,.T.) ;
#1434 = EDGE_CURVE('',#1136,#1138,#666,.T.) ;
#1435 = EDGE_CURVE('',#1135,#1131,#667,.T.) ;
#1436 = EDGE_CURVE('',#1136,#1132,#668,.T.) ;
#1437 = EDGE_CURVE('',#1137,#1134,#669,.T.) ;
#1438 = EDGE_CURVE('',#1138,#1133,#670,.T.) ;
#1439 = ORIENTED_EDGE('',*,*,#1139,.F.) ;
#1440 = ORIENTED_EDGE('',*,*,#1140,.F.) ;
#1441 = ORIENTED_EDGE('',*,*,#1141,.T.) ;
#1442 = ORIENTED_EDGE('',*,*,#1142,.T.) ;
#1443 = ORIENTED_EDGE('',*,*,#1140,.T.) ;
#1444 = ORIENTED_EDGE('',*,*,#1143,.T.) ;
#1445 = ORIENTED_EDGE('',*,*,#1144,.F.) ;
#1446 = ORIENTED_EDGE('',*,*,#1145,.F.) ;
#1447 = ORIENTED_EDGE('',*,*,#1144,.T.) ;
#1448 = ORIENTED_EDGE('',*,*,#1146,.T.) ;
#1449 = ORIENTED_EDGE('',*,*,#1147,.F.) ;
#1450 = ORIENTED_EDGE('',*,*,#1148,.F.) ;
#1451 = ORIENTED_EDGE('',*,*,#1149,.F.) ;
#1452 = ORIENTED_EDGE('',*,*,#1142,.F.) ;
#1453 = ORIENTED_EDGE('',*,*,#1150,.T.) ;
#1454 = ORIENTED_EDGE('',*,*,#1147,.T.) ;
#1455 = ORIENTED_EDGE('',*,*,#1141,.F.) ;
#1456 = ORIENTED_EDGE('',*,*,#1145,.T.) ;
#1457 = ORIENTED_EDGE('',*,*,#1148,.T.) ;
#1458 = ORIENTED_EDGE('',*,*,#1150,.F.) ;
#1459 = ORIENTED_EDGE('',*,*,#1151,.T.) ;
#1460 = ORIENTED_EDGE('',*,*,#1152,.T.) ;
#1461 = ORIENTED_EDGE('',*,*,#1153,.T.) ;
#1462 = ORIENTED_EDGE('',*,*,#1154,.T.) ;
#1463 = ORIENTED_EDGE('',*,*,#1155,.T.) ;
#1464 = ORIENTED_EDGE('',*,*,#1156,.T.) ;
#1465 = ORIENTED_EDGE('',*,*,#1157,.T.) ;
#1466 = ORIENTED_EDGE('',*,*,#1158,.T.) ;
#1467 = ORIENTED_EDGE('',*,*,#1159,.F.) ;
#1468 = ORIENTED_EDGE('',*,*,#1160,.T.) ;
#1469 = ORIENTED_EDGE('',*,*,#1161,.T.) ;
#1470 = ORIENTED_EDGE('',*,*,#1162,.T.) ;
#1471 = ORIENTED_EDGE('',*,*,#1163,.T.) ;
#1472 = ORIENTED_EDGE('',*,*,#1164,.T.) ;
#1473 = ORIENTED_EDGE('',*,*,#1165,.F.) ;
#1474 = ORIENTED_EDGE('',*,*,#1166,.T.) ;
#1475 = ORIENTED_EDGE('',*,*,#1167,.F.) ;
#1476 = ORIENTED_EDGE('',*,*,#1168,.T.) ;
#1477 = ORIENTED_EDGE('',*,*,#1169,.T.) ;
#1478 = ORIENTED_EDGE('',*,*,#1170,.T.) ;
#1479 = ORIENTED_EDGE('',*,*,#1171,.F.) ;
#1480 = ORIENTED_EDGE('',*,*,#1172,.T.) ;
#1481 = ORIENTED_EDGE('',*,*,#1173,.T.) ;
#1482 = ORIENTED_EDGE('',*,*,#1174,.T.) ;
#1483 = ORIENTED_EDGE('',*,*,#1173,.F.) ;
#1484 = ORIENTED_EDGE('',*,*,#1175,.T.) ;
#1485 = ORIENTED_EDGE('',*,*,#1159,.T.) ;
#1486 = ORIENTED_EDGE('',*,*,#1176,.T.) ;
#1487 = ORIENTED_EDGE('',*,*,#1165,.T.) ;
#1488 = ORIENTED_EDGE('',*,*,#1177,.T.) ;
#1489 = ORIENTED_EDGE('',*,*,#1169,.F.) ;
#1490 = ORIENTED_EDGE('',*,*,#1178,.T.) ;
#1491 = ORIENTED_EDGE('',*,*,#1143,.F.) ;
#1492 = ORIENTED_EDGE('',*,*,#1139,.T.) ;
#1493 = ORIENTED_EDGE('',*,*,#1149,.T.) ;
#1494 = ORIENTED_EDGE('',*,*,#1146,.F.) ;
#1495 = ORIENTED_EDGE('',*,*,#1161,.F.) ;
#1496 = ORIENTED_EDGE('',*,*,#1179,.T.) ;
#1497 = ORIENTED_EDGE('',*,*,#1171,.T.) ;
#1498 = ORIENTED_EDGE('',*,*,#1180,.T.) ;
#1499 = ORIENTED_EDGE('',*,*,#1167,.T.) ;
#1500 = ORIENTED_EDGE('',*,*,#1181,.T.) ;
#1501 = ORIENTED_EDGE('',*,*,#1163,.F.) ;
#1502 = ORIENTED_EDGE('',*,*,#1182,.T.) ;
#1503 = ORIENTED_EDGE('',*,*,#1183,.F.) ;
#1504 = ORIENTED_EDGE('',*,*,#1184,.F.) ;
#1505 = ORIENTED_EDGE('',*,*,#1185,.F.) ;
#1506 = ORIENTED_EDGE('',*,*,#1186,.F.) ;
#1507 = ORIENTED_EDGE('',*,*,#1187,.F.) ;
#1508 = ORIENTED_EDGE('',*,*,#1188,.F.) ;
#1509 = ORIENTED_EDGE('',*,*,#1189,.F.) ;
#1510 = ORIENTED_EDGE('',*,*,#1190,.F.) ;
#1511 = ORIENTED_EDGE('',*,*,#1175,.F.) ;
#1512 = ORIENTED_EDGE('',*,*,#1172,.F.) ;
#1513 = ORIENTED_EDGE('',*,*,#1179,.F.) ;
#1514 = ORIENTED_EDGE('',*,*,#1160,.F.) ;
#1515 = ORIENTED_EDGE('',*,*,#1178,.F.) ;
#1516 = ORIENTED_EDGE('',*,*,#1168,.F.) ;
#1517 = ORIENTED_EDGE('',*,*,#1180,.F.) ;
#1518 = ORIENTED_EDGE('',*,*,#1174,.F.) ;
#1519 = ORIENTED_EDGE('',*,*,#1177,.F.) ;
#1520 = ORIENTED_EDGE('',*,*,#1164,.F.) ;
#1521 = ORIENTED_EDGE('',*,*,#1181,.F.) ;
#1522 = ORIENTED_EDGE('',*,*,#1170,.F.) ;
#1523 = ORIENTED_EDGE('',*,*,#1176,.F.) ;
#1524 = ORIENTED_EDGE('',*,*,#1162,.F.) ;
#1525 = ORIENTED_EDGE('',*,*,#1182,.F.) ;
#1526 = ORIENTED_EDGE('',*,*,#1166,.F.) ;
#1527 = ORIENTED_EDGE('',*,*,#1191,.T.) ;
#1528 = ORIENTED_EDGE('',*,*,#1187,.T.) ;
#1529 = ORIENTED_EDGE('',*,*,#1192,.F.) ;
#1530 = ORIENTED_EDGE('',*,*,#1156,.F.) ;
#1531 = ORIENTED_EDGE('',*,*,#1193,.T.) ;
#1532 = ORIENTED_EDGE('',*,*,#1188,.T.) ;
#1533 = ORIENTED_EDGE('',*,*,#1191,.F.) ;
#1534 = ORIENTED_EDGE('',*,*,#1155,.F.) ;
#1535 = ORIENTED_EDGE('',*,*,#1194,.T.) ;
#1536 = ORIENTED_EDGE('',*,*,#1189,.T.) ;
#1537 = ORIENTED_EDGE('',*,*,#1193,.F.) ;
#1538 = ORIENTED_EDGE('',*,*,#1158,.F.) ;
#1539 = ORIENTED_EDGE('',*,*,#1192,.T.) ;
#1540 = ORIENTED_EDGE('',*,*,#1190,.T.) ;
#1541 = ORIENTED_EDGE('',*,*,#1194,.F.) ;
#1542 = ORIENTED_EDGE('',*,*,#1157,.F.) ;
#1543 = ORIENTED_EDGE('',*,*,#1195,.T.) ;
#1544 = ORIENTED_EDGE('',*,*,#1183,.T.) ;
#1545 = ORIENTED_EDGE('',*,*,#1196,.F.) ;
#1546 = ORIENTED_EDGE('',*,*,#1152,.F.) ;
#1547 = ORIENTED_EDGE('',*,*,#1197,.T.) ;
#1548 = ORIENTED_EDGE('',*,*,#1184,.T.) ;
#1549 = ORIENTED_EDGE('',*,*,#1195,.F.) ;
#1550 = ORIENTED_EDGE('',*,*,#1151,.F.) ;
#1551 = ORIENTED_EDGE('',*,*,#1198,.T.) ;
#1552 = ORIENTED_EDGE('',*,*,#1185,.T.) ;
#1553 = ORIENTED_EDGE('',*,*,#1197,.F.) ;
#1554 = ORIENTED_EDGE('',*,*,#1154,.F.) ;
#1555 = ORIENTED_EDGE('',*,*,#1196,.T.) ;
#1556 = ORIENTED_EDGE('',*,*,#1186,.T.) ;
#1557 = ORIENTED_EDGE('',*,*,#1198,.F.) ;
#1558 = ORIENTED_EDGE('',*,*,#1153,.F.) ;
#1559 = ORIENTED_EDGE('',*,*,#1199,.F.) ;
#1560 = ORIENTED_EDGE('',*,*,#1200,.F.) ;
#1561 = ORIENTED_EDGE('',*,*,#1201,.T.) ;
#1562 = ORIENTED_EDGE('',*,*,#1202,.T.) ;
#1563 = ORIENTED_EDGE('',*,*,#1200,.T.) ;
#1564 = ORIENTED_EDGE('',*,*,#1203,.T.) ;
#1565 = ORIENTED_EDGE('',*,*,#1204,.F.) ;
#1566 = ORIENTED_EDGE('',*,*,#1205,.F.) ;
#1567 = ORIENTED_EDGE('',*,*,#1204,.T.) ;
#1568 = ORIENTED_EDGE('',*,*,#1206,.T.) ;
#1569 = ORIENTED_EDGE('',*,*,#1207,.F.) ;
#1570 = ORIENTED_EDGE('',*,*,#1208,.F.) ;
#1571 = ORIENTED_EDGE('',*,*,#1209,.F.) ;
#1572 = ORIENTED_EDGE('',*,*,#1202,.F.) ;
#1573 = ORIENTED_EDGE('',*,*,#1210,.T.) ;
#1574 = ORIENTED_EDGE('',*,*,#1207,.T.) ;
#1575 = ORIENTED_EDGE('',*,*,#1201,.F.) ;
#1576 = ORIENTED_EDGE('',*,*,#1205,.T.) ;
#1577 = ORIENTED_EDGE('',*,*,#1208,.T.) ;
#1578 = ORIENTED_EDGE('',*,*,#1210,.F.) ;
#1579 = ORIENTED_EDGE('',*,*,#1211,.T.) ;
#1580 = ORIENTED_EDGE('',*,*,#1212,.T.) ;
#1581 = ORIENTED_EDGE('',*,*,#1213,.T.) ;
#1582 = ORIENTED_EDGE('',*,*,#1214,.T.) ;
#1583 = ORIENTED_EDGE('',*,*,#1215,.T.) ;
#1584 = ORIENTED_EDGE('',*,*,#1216,.T.) ;
#1585 = ORIENTED_EDGE('',*,*,#1217,.T.) ;
#1586 = ORIENTED_EDGE('',*,*,#1218,.T.) ;
#1587 = ORIENTED_EDGE('',*,*,#1219,.F.) ;
#1588 = ORIENTED_EDGE('',*,*,#1220,.T.) ;
#1589 = ORIENTED_EDGE('',*,*,#1221,.T.) ;
#1590 = ORIENTED_EDGE('',*,*,#1222,.T.) ;
#1591 = ORIENTED_EDGE('',*,*,#1223,.T.) ;
#1592 = ORIENTED_EDGE('',*,*,#1224,.T.) ;
#1593 = ORIENTED_EDGE('',*,*,#1225,.F.) ;
#1594 = ORIENTED_EDGE('',*,*,#1226,.T.) ;
#1595 = ORIENTED_EDGE('',*,*,#1227,.F.) ;
#1596 = ORIENTED_EDGE('',*,*,#1228,.T.) ;
#1597 = ORIENTED_EDGE('',*,*,#1229,.T.) ;
#1598 = ORIENTED_EDGE('',*,*,#1230,.T.) ;
#1599 = ORIENTED_EDGE('',*,*,#1231,.F.) ;
#1600 = ORIENTED_EDGE('',*,*,#1232,.T.) ;
#1601 = ORIENTED_EDGE('',*,*,#1233,.T.) ;
#1602 = ORIENTED_EDGE('',*,*,#1234,.T.) ;
#1603 = ORIENTED_EDGE('',*,*,#1233,.F.) ;
#1604 = ORIENTED_EDGE('',*,*,#1235,.T.) ;
#1605 = ORIENTED_EDGE('',*,*,#1219,.T.) ;
#1606 = ORIENTED_EDGE('',*,*,#1236,.T.) ;
#1607 = ORIENTED_EDGE('',*,*,#1225,.T.) ;
#1608 = ORIENTED_EDGE('',*,*,#1237,.T.) ;
#1609 = ORIENTED_EDGE('',*,*,#1229,.F.) ;
#1610 = ORIENTED_EDGE('',*,*,#1238,.T.) ;
#1611 = ORIENTED_EDGE('',*,*,#1203,.F.) ;
#1612 = ORIENTED_EDGE('',*,*,#1199,.T.) ;
#1613 = ORIENTED_EDGE('',*,*,#1209,.T.) ;
#1614 = ORIENTED_EDGE('',*,*,#1206,.F.) ;
#1615 = ORIENTED_EDGE('',*,*,#1221,.F.) ;
#1616 = ORIENTED_EDGE('',*,*,#1239,.T.) ;
#1617 = ORIENTED_EDGE('',*,*,#1231,.T.) ;
#1618 = ORIENTED_EDGE('',*,*,#1240,.T.) ;
#1619 = ORIENTED_EDGE('',*,*,#1227,.T.) ;
#1620 = ORIENTED_EDGE('',*,*,#1241,.T.) ;
#1621 = ORIENTED_EDGE('',*,*,#1223,.F.) ;
#1622 = ORIENTED_EDGE('',*,*,#1242,.T.) ;
#1623 = ORIENTED_EDGE('',*,*,#1243,.F.) ;
#1624 = ORIENTED_EDGE('',*,*,#1244,.F.) ;
#1625 = ORIENTED_EDGE('',*,*,#1245,.F.) ;
#1626 = ORIENTED_EDGE('',*,*,#1246,.F.) ;
#1627 = ORIENTED_EDGE('',*,*,#1247,.F.) ;
#1628 = ORIENTED_EDGE('',*,*,#1248,.F.) ;
#1629 = ORIENTED_EDGE('',*,*,#1249,.F.) ;
#1630 = ORIENTED_EDGE('',*,*,#1250,.F.) ;
#1631 = ORIENTED_EDGE('',*,*,#1235,.F.) ;
#1632 = ORIENTED_EDGE('',*,*,#1232,.F.) ;
#1633 = ORIENTED_EDGE('',*,*,#1239,.F.) ;
#1634 = ORIENTED_EDGE('',*,*,#1220,.F.) ;
#1635 = ORIENTED_EDGE('',*,*,#1238,.F.) ;
#1636 = ORIENTED_EDGE('',*,*,#1228,.F.) ;
#1637 = ORIENTED_EDGE('',*,*,#1240,.F.) ;
#1638 = ORIENTED_EDGE('',*,*,#1234,.F.) ;
#1639 = ORIENTED_EDGE('',*,*,#1237,.F.) ;
#1640 = ORIENTED_EDGE('',*,*,#1224,.F.) ;
#1641 = ORIENTED_EDGE('',*,*,#1241,.F.) ;
#1642 = ORIENTED_EDGE('',*,*,#1230,.F.) ;
#1643 = ORIENTED_EDGE('',*,*,#1236,.F.) ;
#1644 = ORIENTED_EDGE('',*,*,#1222,.F.) ;
#1645 = ORIENTED_EDGE('',*,*,#1242,.F.) ;
#1646 = ORIENTED_EDGE('',*,*,#1226,.F.) ;
#1647 = ORIENTED_EDGE('',*,*,#1251,.T.) ;
#1648 = ORIENTED_EDGE('',*,*,#1247,.T.) ;
#1649 = ORIENTED_EDGE('',*,*,#1252,.F.) ;
#1650 = ORIENTED_EDGE('',*,*,#1216,.F.) ;
#1651 = ORIENTED_EDGE('',*,*,#1253,.T.) ;
#1652 = ORIENTED_EDGE('',*,*,#1248,.T.) ;
#1653 = ORIENTED_EDGE('',*,*,#1251,.F.) ;
#1654 = ORIENTED_EDGE('',*,*,#1215,.F.) ;
#1655 = ORIENTED_EDGE('',*,*,#1254,.T.) ;
#1656 = ORIENTED_EDGE('',*,*,#1249,.T.) ;
#1657 = ORIENTED_EDGE('',*,*,#1253,.F.) ;
#1658 = ORIENTED_EDGE('',*,*,#1218,.F.) ;
#1659 = ORIENTED_EDGE('',*,*,#1252,.T.) ;
#1660 = ORIENTED_EDGE('',*,*,#1250,.T.) ;
#1661 = ORIENTED_EDGE('',*,*,#1254,.F.) ;
#1662 = ORIENTED_EDGE('',*,*,#1217,.F.) ;
#1663 = ORIENTED_EDGE('',*,*,#1255,.T.) ;
#1664 = ORIENTED_EDGE('',*,*,#1243,.T.) ;
#1665 = ORIENTED_EDGE('',*,*,#1256,.F.) ;
#1666 = ORIENTED_EDGE('',*,*,#1212,.F.) ;
#1667 = ORIENTED_EDGE('',*,*,#1257,.T.) ;
#1668 = ORIENTED_EDGE('',*,*,#1244,.T.) ;
#1669 = ORIENTED_EDGE('',*,*,#1255,.F.) ;
#1670 = ORIENTED_EDGE('',*,*,#1211,.F.) ;
#1671 = ORIENTED_EDGE('',*,*,#1258,.T.) ;
#1672 = ORIENTED_EDGE('',*,*,#1245,.T.) ;
#1673 = ORIENTED_EDGE('',*,*,#1257,.F.) ;
#1674 = ORIENTED_EDGE('',*,*,#1214,.F.) ;
#1675 = ORIENTED_EDGE('',*,*,#1256,.T.) ;
#1676 = ORIENTED_EDGE('',*,*,#1246,.T.) ;
#1677 = ORIENTED_EDGE('',*,*,#1258,.F.) ;
#1678 = ORIENTED_EDGE('',*,*,#1213,.F.) ;
#1679 = ORIENTED_EDGE('',*,*,#1259,.F.) ;
#1680 = ORIENTED_EDGE('',*,*,#1260,.F.) ;
#1681 = ORIENTED_EDGE('',*,*,#1261,.T.) ;
#1682 = ORIENTED_EDGE('',*,*,#1262,.T.) ;
#1683 = ORIENTED_EDGE('',*,*,#1260,.T.) ;
#1684 = ORIENTED_EDGE('',*,*,#1263,.T.) ;
#1685 = ORIENTED_EDGE('',*,*,#1264,.F.) ;
#1686 = ORIENTED_EDGE('',*,*,#1265,.F.) ;
#1687 = ORIENTED_EDGE('',*,*,#1264,.T.) ;
#1688 = ORIENTED_EDGE('',*,*,#1266,.T.) ;
#1689 = ORIENTED_EDGE('',*,*,#1267,.F.) ;
#1690 = ORIENTED_EDGE('',*,*,#1268,.F.) ;
#1691 = ORIENTED_EDGE('',*,*,#1269,.F.) ;
#1692 = ORIENTED_EDGE('',*,*,#1262,.F.) ;
#1693 = ORIENTED_EDGE('',*,*,#1270,.T.) ;
#1694 = ORIENTED_EDGE('',*,*,#1267,.T.) ;
#1695 = ORIENTED_EDGE('',*,*,#1261,.F.) ;
#1696 = ORIENTED_EDGE('',*,*,#1265,.T.) ;
#1697 = ORIENTED_EDGE('',*,*,#1268,.T.) ;
#1698 = ORIENTED_EDGE('',*,*,#1270,.F.) ;
#1699 = ORIENTED_EDGE('',*,*,#1271,.T.) ;
#1700 = ORIENTED_EDGE('',*,*,#1272,.T.) ;
#1701 = ORIENTED_EDGE('',*,*,#1273,.T.) ;
#1702 = ORIENTED_EDGE('',*,*,#1274,.T.) ;
#1703 = ORIENTED_EDGE('',*,*,#1275,.F.) ;
#1704 = ORIENTED_EDGE('',*,*,#1276,.T.) ;
#1705 = ORIENTED_EDGE('',*,*,#1277,.T.) ;
#1706 = ORIENTED_EDGE('',*,*,#1278,.T.) ;
#1707 = ORIENTED_EDGE('',*,*,#1279,.T.) ;
#1708 = ORIENTED_EDGE('',*,*,#1280,.T.) ;
#1709 = ORIENTED_EDGE('',*,*,#1281,.F.) ;
#1710 = ORIENTED_EDGE('',*,*,#1282,.T.) ;
#1711 = ORIENTED_EDGE('',*,*,#1283,.F.) ;
#1712 = ORIENTED_EDGE('',*,*,#1284,.T.) ;
#1713 = ORIENTED_EDGE('',*,*,#1285,.T.) ;
#1714 = ORIENTED_EDGE('',*,*,#1286,.T.) ;
#1715 = ORIENTED_EDGE('',*,*,#1287,.F.) ;
#1716 = ORIENTED_EDGE('',*,*,#1288,.T.) ;
#1717 = ORIENTED_EDGE('',*,*,#1289,.T.) ;
#1718 = ORIENTED_EDGE('',*,*,#1290,.T.) ;
#1719 = ORIENTED_EDGE('',*,*,#1289,.F.) ;
#1720 = ORIENTED_EDGE('',*,*,#1291,.T.) ;
#1721 = ORIENTED_EDGE('',*,*,#1275,.T.) ;
#1722 = ORIENTED_EDGE('',*,*,#1292,.T.) ;
#1723 = ORIENTED_EDGE('',*,*,#1281,.T.) ;
#1724 = ORIENTED_EDGE('',*,*,#1293,.T.) ;
#1725 = ORIENTED_EDGE('',*,*,#1285,.F.) ;
#1726 = ORIENTED_EDGE('',*,*,#1294,.T.) ;
#1727 = ORIENTED_EDGE('',*,*,#1263,.F.) ;
#1728 = ORIENTED_EDGE('',*,*,#1259,.T.) ;
#1729 = ORIENTED_EDGE('',*,*,#1269,.T.) ;
#1730 = ORIENTED_EDGE('',*,*,#1266,.F.) ;
#1731 = ORIENTED_EDGE('',*,*,#1277,.F.) ;
#1732 = ORIENTED_EDGE('',*,*,#1295,.T.) ;
#1733 = ORIENTED_EDGE('',*,*,#1287,.T.) ;
#1734 = ORIENTED_EDGE('',*,*,#1296,.T.) ;
#1735 = ORIENTED_EDGE('',*,*,#1283,.T.) ;
#1736 = ORIENTED_EDGE('',*,*,#1297,.T.) ;
#1737 = ORIENTED_EDGE('',*,*,#1279,.F.) ;
#1738 = ORIENTED_EDGE('',*,*,#1298,.T.) ;
#1739 = ORIENTED_EDGE('',*,*,#1299,.F.) ;
#1740 = ORIENTED_EDGE('',*,*,#1300,.F.) ;
#1741 = ORIENTED_EDGE('',*,*,#1301,.F.) ;
#1742 = ORIENTED_EDGE('',*,*,#1302,.F.) ;
#1743 = ORIENTED_EDGE('',*,*,#1291,.F.) ;
#1744 = ORIENTED_EDGE('',*,*,#1288,.F.) ;
#1745 = ORIENTED_EDGE('',*,*,#1295,.F.) ;
#1746 = ORIENTED_EDGE('',*,*,#1276,.F.) ;
#1747 = ORIENTED_EDGE('',*,*,#1294,.F.) ;
#1748 = ORIENTED_EDGE('',*,*,#1284,.F.) ;
#1749 = ORIENTED_EDGE('',*,*,#1296,.F.) ;
#1750 = ORIENTED_EDGE('',*,*,#1290,.F.) ;
#1751 = ORIENTED_EDGE('',*,*,#1293,.F.) ;
#1752 = ORIENTED_EDGE('',*,*,#1280,.F.) ;
#1753 = ORIENTED_EDGE('',*,*,#1297,.F.) ;
#1754 = ORIENTED_EDGE('',*,*,#1286,.F.) ;
#1755 = ORIENTED_EDGE('',*,*,#1292,.F.) ;
#1756 = ORIENTED_EDGE('',*,*,#1278,.F.) ;
#1757 = ORIENTED_EDGE('',*,*,#1298,.F.) ;
#1758 = ORIENTED_EDGE('',*,*,#1282,.F.) ;
#1759 = ORIENTED_EDGE('',*,*,#1303,.T.) ;
#1760 = ORIENTED_EDGE('',*,*,#1299,.T.) ;
#1761 = ORIENTED_EDGE('',*,*,#1304,.F.) ;
#1762 = ORIENTED_EDGE('',*,*,#1272,.F.) ;
#1763 = ORIENTED_EDGE('',*,*,#1305,.T.) ;
#1764 = ORIENTED_EDGE('',*,*,#1300,.T.) ;
#1765 = ORIENTED_EDGE('',*,*,#1303,.F.) ;
#1766 = ORIENTED_EDGE('',*,*,#1271,.F.) ;
#1767 = ORIENTED_EDGE('',*,*,#1306,.T.) ;
#1768 = ORIENTED_EDGE('',*,*,#1301,.T.) ;
#1769 = ORIENTED_EDGE('',*,*,#1305,.F.) ;
#1770 = ORIENTED_EDGE('',*,*,#1274,.F.) ;
#1771 = ORIENTED_EDGE('',*,*,#1304,.T.) ;
#1772 = ORIENTED_EDGE('',*,*,#1302,.T.) ;
#1773 = ORIENTED_EDGE('',*,*,#1306,.F.) ;
#1774 = ORIENTED_EDGE('',*,*,#1273,.F.) ;
#1775 = ORIENTED_EDGE('',*,*,#1307,.F.) ;
#1776 = ORIENTED_EDGE('',*,*,#1308,.F.) ;
#1777 = ORIENTED_EDGE('',*,*,#1309,.T.) ;
#1778 = ORIENTED_EDGE('',*,*,#1310,.T.) ;
#1779 = ORIENTED_EDGE('',*,*,#1308,.T.) ;
#1780 = ORIENTED_EDGE('',*,*,#1311,.T.) ;
#1781 = ORIENTED_EDGE('',*,*,#1312,.F.) ;
#1782 = ORIENTED_EDGE('',*,*,#1313,.F.) ;
#1783 = ORIENTED_EDGE('',*,*,#1312,.T.) ;
#1784 = ORIENTED_EDGE('',*,*,#1314,.T.) ;
#1785 = ORIENTED_EDGE('',*,*,#1315,.F.) ;
#1786 = ORIENTED_EDGE('',*,*,#1316,.F.) ;
#1787 = ORIENTED_EDGE('',*,*,#1317,.F.) ;
#1788 = ORIENTED_EDGE('',*,*,#1310,.F.) ;
#1789 = ORIENTED_EDGE('',*,*,#1318,.T.) ;
#1790 = ORIENTED_EDGE('',*,*,#1315,.T.) ;
#1791 = ORIENTED_EDGE('',*,*,#1309,.F.) ;
#1792 = ORIENTED_EDGE('',*,*,#1313,.T.) ;
#1793 = ORIENTED_EDGE('',*,*,#1316,.T.) ;
#1794 = ORIENTED_EDGE('',*,*,#1318,.F.) ;
#1795 = ORIENTED_EDGE('',*,*,#1319,.F.) ;
#1796 = ORIENTED_EDGE('',*,*,#1320,.T.) ;
#1797 = ORIENTED_EDGE('',*,*,#1321,.T.) ;
#1798 = ORIENTED_EDGE('',*,*,#1322,.T.) ;
#1799 = ORIENTED_EDGE('',*,*,#1323,.T.) ;
#1800 = ORIENTED_EDGE('',*,*,#1324,.T.) ;
#1801 = ORIENTED_EDGE('',*,*,#1325,.F.) ;
#1802 = ORIENTED_EDGE('',*,*,#1326,.T.) ;
#1803 = ORIENTED_EDGE('',*,*,#1327,.F.) ;
#1804 = ORIENTED_EDGE('',*,*,#1328,.T.) ;
#1805 = ORIENTED_EDGE('',*,*,#1329,.T.) ;
#1806 = ORIENTED_EDGE('',*,*,#1330,.T.) ;
#1807 = ORIENTED_EDGE('',*,*,#1331,.F.) ;
#1808 = ORIENTED_EDGE('',*,*,#1332,.T.) ;
#1809 = ORIENTED_EDGE('',*,*,#1333,.T.) ;
#1810 = ORIENTED_EDGE('',*,*,#1334,.T.) ;
#1811 = ORIENTED_EDGE('',*,*,#1333,.F.) ;
#1812 = ORIENTED_EDGE('',*,*,#1335,.T.) ;
#1813 = ORIENTED_EDGE('',*,*,#1319,.T.) ;
#1814 = ORIENTED_EDGE('',*,*,#1336,.T.) ;
#1815 = ORIENTED_EDGE('',*,*,#1325,.T.) ;
#1816 = ORIENTED_EDGE('',*,*,#1337,.T.) ;
#1817 = ORIENTED_EDGE('',*,*,#1329,.F.) ;
#1818 = ORIENTED_EDGE('',*,*,#1338,.T.) ;
#1819 = ORIENTED_EDGE('',*,*,#1311,.F.) ;
#1820 = ORIENTED_EDGE('',*,*,#1307,.T.) ;
#1821 = ORIENTED_EDGE('',*,*,#1317,.T.) ;
#1822 = ORIENTED_EDGE('',*,*,#1314,.F.) ;
#1823 = ORIENTED_EDGE('',*,*,#1321,.F.) ;
#1824 = ORIENTED_EDGE('',*,*,#1339,.T.) ;
#1825 = ORIENTED_EDGE('',*,*,#1331,.T.) ;
#1826 = ORIENTED_EDGE('',*,*,#1340,.T.) ;
#1827 = ORIENTED_EDGE('',*,*,#1327,.T.) ;
#1828 = ORIENTED_EDGE('',*,*,#1341,.T.) ;
#1829 = ORIENTED_EDGE('',*,*,#1323,.F.) ;
#1830 = ORIENTED_EDGE('',*,*,#1342,.T.) ;
#1831 = ORIENTED_EDGE('',*,*,#1335,.F.) ;
#1832 = ORIENTED_EDGE('',*,*,#1332,.F.) ;
#1833 = ORIENTED_EDGE('',*,*,#1339,.F.) ;
#1834 = ORIENTED_EDGE('',*,*,#1320,.F.) ;
#1835 = ORIENTED_EDGE('',*,*,#1338,.F.) ;
#1836 = ORIENTED_EDGE('',*,*,#1328,.F.) ;
#1837 = ORIENTED_EDGE('',*,*,#1340,.F.) ;
#1838 = ORIENTED_EDGE('',*,*,#1334,.F.) ;
#1839 = ORIENTED_EDGE('',*,*,#1337,.F.) ;
#1840 = ORIENTED_EDGE('',*,*,#1324,.F.) ;
#1841 = ORIENTED_EDGE('',*,*,#1341,.F.) ;
#1842 = ORIENTED_EDGE('',*,*,#1330,.F.) ;
#1843 = ORIENTED_EDGE('',*,*,#1336,.F.) ;
#1844 = ORIENTED_EDGE('',*,*,#1322,.F.) ;
#1845 = ORIENTED_EDGE('',*,*,#1342,.F.) ;
#1846 = ORIENTED_EDGE('',*,*,#1326,.F.) ;
#1847 = ORIENTED_EDGE('',*,*,#1343,.F.) ;
#1848 = ORIENTED_EDGE('',*,*,#1344,.T.) ;
#1849 = ORIENTED_EDGE('',*,*,#1345,.F.) ;
#1850 = ORIENTED_EDGE('',*,*,#1346,.F.) ;
#1851 = ORIENTED_EDGE('',*,*,#1347,.F.) ;
#1852 = ORIENTED_EDGE('',*,*,#1346,.T.) ;
#1853 = ORIENTED_EDGE('',*,*,#1348,.F.) ;
#1854 = ORIENTED_EDGE('',*,*,#1349,.F.) ;
#1855 = ORIENTED_EDGE('',*,*,#1350,.F.) ;
#1856 = ORIENTED_EDGE('',*,*,#1349,.T.) ;
#1857 = ORIENTED_EDGE('',*,*,#1351,.F.) ;
#1858 = ORIENTED_EDGE('',*,*,#1352,.F.) ;
#1859 = ORIENTED_EDGE('',*,*,#1353,.F.) ;
#1860 = ORIENTED_EDGE('',*,*,#1352,.T.) ;
#1861 = ORIENTED_EDGE('',*,*,#1354,.F.) ;
#1862 = ORIENTED_EDGE('',*,*,#1344,.F.) ;
#1863 = ORIENTED_EDGE('',*,*,#1355,.T.) ;
#1864 = ORIENTED_EDGE('',*,*,#1356,.T.) ;
#1865 = ORIENTED_EDGE('',*,*,#1357,.T.) ;
#1866 = ORIENTED_EDGE('',*,*,#1358,.T.) ;
#1867 = ORIENTED_EDGE('',*,*,#1348,.T.) ;
#1868 = ORIENTED_EDGE('',*,*,#1345,.T.) ;
#1869 = ORIENTED_EDGE('',*,*,#1354,.T.) ;
#1870 = ORIENTED_EDGE('',*,*,#1351,.T.) ;
#1871 = ORIENTED_EDGE('',*,*,#1359,.F.) ;
#1872 = ORIENTED_EDGE('',*,*,#1360,.F.) ;
#1873 = ORIENTED_EDGE('',*,*,#1361,.F.) ;
#1874 = ORIENTED_EDGE('',*,*,#1362,.F.) ;
#1875 = ORIENTED_EDGE('',*,*,#1363,.T.) ;
#1876 = ORIENTED_EDGE('',*,*,#1364,.T.) ;
#1877 = ORIENTED_EDGE('',*,*,#1365,.T.) ;
#1878 = ORIENTED_EDGE('',*,*,#1366,.T.) ;
#1879 = ORIENTED_EDGE('',*,*,#1359,.T.) ;
#1880 = ORIENTED_EDGE('',*,*,#1367,.F.) ;
#1881 = ORIENTED_EDGE('',*,*,#1355,.F.) ;
#1882 = ORIENTED_EDGE('',*,*,#1368,.T.) ;
#1883 = ORIENTED_EDGE('',*,*,#1362,.T.) ;
#1884 = ORIENTED_EDGE('',*,*,#1369,.F.) ;
#1885 = ORIENTED_EDGE('',*,*,#1356,.F.) ;
#1886 = ORIENTED_EDGE('',*,*,#1367,.T.) ;
#1887 = ORIENTED_EDGE('',*,*,#1361,.T.) ;
#1888 = ORIENTED_EDGE('',*,*,#1370,.F.) ;
#1889 = ORIENTED_EDGE('',*,*,#1357,.F.) ;
#1890 = ORIENTED_EDGE('',*,*,#1369,.T.) ;
#1891 = ORIENTED_EDGE('',*,*,#1360,.T.) ;
#1892 = ORIENTED_EDGE('',*,*,#1368,.F.) ;
#1893 = ORIENTED_EDGE('',*,*,#1358,.F.) ;
#1894 = ORIENTED_EDGE('',*,*,#1370,.T.) ;
#1895 = ORIENTED_EDGE('',*,*,#1371,.T.) ;
#1896 = ORIENTED_EDGE('',*,*,#1363,.F.) ;
#1897 = ORIENTED_EDGE('',*,*,#1372,.F.) ;
#1898 = ORIENTED_EDGE('',*,*,#1373,.T.) ;
#1899 = ORIENTED_EDGE('',*,*,#1374,.T.) ;
#1900 = ORIENTED_EDGE('',*,*,#1364,.F.) ;
#1901 = ORIENTED_EDGE('',*,*,#1371,.F.) ;
#1902 = ORIENTED_EDGE('',*,*,#1375,.T.) ;
#1903 = ORIENTED_EDGE('',*,*,#1376,.T.) ;
#1904 = ORIENTED_EDGE('',*,*,#1365,.F.) ;
#1905 = ORIENTED_EDGE('',*,*,#1374,.F.) ;
#1906 = ORIENTED_EDGE('',*,*,#1377,.T.) ;
#1907 = ORIENTED_EDGE('',*,*,#1372,.T.) ;
#1908 = ORIENTED_EDGE('',*,*,#1366,.F.) ;
#1909 = ORIENTED_EDGE('',*,*,#1376,.F.) ;
#1910 = ORIENTED_EDGE('',*,*,#1378,.T.) ;
#1911 = ORIENTED_EDGE('',*,*,#1379,.T.) ;
#1912 = ORIENTED_EDGE('',*,*,#1380,.T.) ;
#1913 = ORIENTED_EDGE('',*,*,#1381,.T.) ;
#1914 = ORIENTED_EDGE('',*,*,#1382,.T.) ;
#1915 = ORIENTED_EDGE('',*,*,#1375,.F.) ;
#1916 = ORIENTED_EDGE('',*,*,#1373,.F.) ;
#1917 = ORIENTED_EDGE('',*,*,#1378,.F.) ;
#1918 = ORIENTED_EDGE('',*,*,#1377,.F.) ;
#1919 = ORIENTED_EDGE('',*,*,#1383,.F.) ;
#1920 = ORIENTED_EDGE('',*,*,#1384,.F.) ;
#1921 = ORIENTED_EDGE('',*,*,#1385,.F.) ;
#1922 = ORIENTED_EDGE('',*,*,#1386,.F.) ;
#1923 = ORIENTED_EDGE('',*,*,#1353,.T.) ;
#1924 = ORIENTED_EDGE('',*,*,#1343,.T.) ;
#1925 = ORIENTED_EDGE('',*,*,#1347,.T.) ;
#1926 = ORIENTED_EDGE('',*,*,#1350,.T.) ;
#1927 = ORIENTED_EDGE('',*,*,#1379,.F.) ;
#1928 = ORIENTED_EDGE('',*,*,#1387,.F.) ;
#1929 = ORIENTED_EDGE('',*,*,#1383,.T.) ;
#1930 = ORIENTED_EDGE('',*,*,#1388,.T.) ;
#1931 = ORIENTED_EDGE('',*,*,#1382,.F.) ;
#1932 = ORIENTED_EDGE('',*,*,#1389,.F.) ;
#1933 = ORIENTED_EDGE('',*,*,#1384,.T.) ;
#1934 = ORIENTED_EDGE('',*,*,#1387,.T.) ;
#1935 = ORIENTED_EDGE('',*,*,#1381,.F.) ;
#1936 = ORIENTED_EDGE('',*,*,#1390,.F.) ;
#1937 = ORIENTED_EDGE('',*,*,#1385,.T.) ;
#1938 = ORIENTED_EDGE('',*,*,#1389,.T.) ;
#1939 = ORIENTED_EDGE('',*,*,#1380,.F.) ;
#1940 = ORIENTED_EDGE('',*,*,#1388,.F.) ;
#1941 = ORIENTED_EDGE('',*,*,#1386,.T.) ;
#1942 = ORIENTED_EDGE('',*,*,#1390,.T.) ;
#1943 = ORIENTED_EDGE('',*,*,#1391,.F.) ;
#1944 = ORIENTED_EDGE('',*,*,#1392,.T.) ;
#1945 = ORIENTED_EDGE('',*,*,#1393,.F.) ;
#1946 = ORIENTED_EDGE('',*,*,#1394,.F.) ;
#1947 = ORIENTED_EDGE('',*,*,#1395,.F.) ;
#1948 = ORIENTED_EDGE('',*,*,#1394,.T.) ;
#1949 = ORIENTED_EDGE('',*,*,#1396,.F.) ;
#1950 = ORIENTED_EDGE('',*,*,#1397,.F.) ;
#1951 = ORIENTED_EDGE('',*,*,#1398,.F.) ;
#1952 = ORIENTED_EDGE('',*,*,#1397,.T.) ;
#1953 = ORIENTED_EDGE('',*,*,#1399,.F.) ;
#1954 = ORIENTED_EDGE('',*,*,#1400,.F.) ;
#1955 = ORIENTED_EDGE('',*,*,#1401,.F.) ;
#1956 = ORIENTED_EDGE('',*,*,#1400,.T.) ;
#1957 = ORIENTED_EDGE('',*,*,#1402,.F.) ;
#1958 = ORIENTED_EDGE('',*,*,#1392,.F.) ;
#1959 = ORIENTED_EDGE('',*,*,#1403,.T.) ;
#1960 = ORIENTED_EDGE('',*,*,#1404,.T.) ;
#1961 = ORIENTED_EDGE('',*,*,#1405,.T.) ;
#1962 = ORIENTED_EDGE('',*,*,#1406,.T.) ;
#1963 = ORIENTED_EDGE('',*,*,#1396,.T.) ;
#1964 = ORIENTED_EDGE('',*,*,#1393,.T.) ;
#1965 = ORIENTED_EDGE('',*,*,#1402,.T.) ;
#1966 = ORIENTED_EDGE('',*,*,#1399,.T.) ;
#1967 = ORIENTED_EDGE('',*,*,#1407,.F.) ;
#1968 = ORIENTED_EDGE('',*,*,#1408,.F.) ;
#1969 = ORIENTED_EDGE('',*,*,#1409,.F.) ;
#1970 = ORIENTED_EDGE('',*,*,#1410,.F.) ;
#1971 = ORIENTED_EDGE('',*,*,#1411,.T.) ;
#1972 = ORIENTED_EDGE('',*,*,#1412,.T.) ;
#1973 = ORIENTED_EDGE('',*,*,#1413,.T.) ;
#1974 = ORIENTED_EDGE('',*,*,#1414,.T.) ;
#1975 = ORIENTED_EDGE('',*,*,#1407,.T.) ;
#1976 = ORIENTED_EDGE('',*,*,#1415,.F.) ;
#1977 = ORIENTED_EDGE('',*,*,#1403,.F.) ;
#1978 = ORIENTED_EDGE('',*,*,#1416,.T.) ;
#1979 = ORIENTED_EDGE('',*,*,#1410,.T.) ;
#1980 = ORIENTED_EDGE('',*,*,#1417,.F.) ;
#1981 = ORIENTED_EDGE('',*,*,#1404,.F.) ;
#1982 = ORIENTED_EDGE('',*,*,#1415,.T.) ;
#1983 = ORIENTED_EDGE('',*,*,#1409,.T.) ;
#1984 = ORIENTED_EDGE('',*,*,#1418,.F.) ;
#1985 = ORIENTED_EDGE('',*,*,#1405,.F.) ;
#1986 = ORIENTED_EDGE('',*,*,#1417,.T.) ;
#1987 = ORIENTED_EDGE('',*,*,#1408,.T.) ;
#1988 = ORIENTED_EDGE('',*,*,#1416,.F.) ;
#1989 = ORIENTED_EDGE('',*,*,#1406,.F.) ;
#1990 = ORIENTED_EDGE('',*,*,#1418,.T.) ;
#1991 = ORIENTED_EDGE('',*,*,#1419,.T.) ;
#1992 = ORIENTED_EDGE('',*,*,#1411,.F.) ;
#1993 = ORIENTED_EDGE('',*,*,#1420,.F.) ;
#1994 = ORIENTED_EDGE('',*,*,#1421,.T.) ;
#1995 = ORIENTED_EDGE('',*,*,#1422,.T.) ;
#1996 = ORIENTED_EDGE('',*,*,#1412,.F.) ;
#1997 = ORIENTED_EDGE('',*,*,#1419,.F.) ;
#1998 = ORIENTED_EDGE('',*,*,#1423,.T.) ;
#1999 = ORIENTED_EDGE('',*,*,#1424,.T.) ;
#2000 = ORIENTED_EDGE('',*,*,#1413,.F.) ;
#2001 = ORIENTED_EDGE('',*,*,#1422,.F.) ;
#2002 = ORIENTED_EDGE('',*,*,#1425,.T.) ;
#2003 = ORIENTED_EDGE('',*,*,#1420,.T.) ;
#2004 = ORIENTED_EDGE('',*,*,#1414,.F.) ;
#2005 = ORIENTED_EDGE('',*,*,#1424,.F.) ;
#2006 = ORIENTED_EDGE('',*,*,#1426,.T.) ;
#2007 = ORIENTED_EDGE('',*,*,#1427,.T.) ;
#2008 = ORIENTED_EDGE('',*,*,#1428,.T.) ;
#2009 = ORIENTED_EDGE('',*,*,#1429,.T.) ;
#2010 = ORIENTED_EDGE('',*,*,#1430,.T.) ;
#2011 = ORIENTED_EDGE('',*,*,#1423,.F.) ;
#2012 = ORIENTED_EDGE('',*,*,#1421,.F.) ;
#2013 = ORIENTED_EDGE('',*,*,#1426,.F.) ;
#2014 = ORIENTED_EDGE('',*,*,#1425,.F.) ;
#2015 = ORIENTED_EDGE('',*,*,#1431,.F.) ;
#2016 = ORIENTED_EDGE('',*,*,#1432,.F.) ;
#2017 = ORIENTED_EDGE('',*,*,#1433,.F.) ;
#2018 = ORIENTED_EDGE('',*,*,#1434,.F.) ;
#2019 = ORIENTED_EDGE('',*,*,#1401,.T.) ;
#2020 = ORIENTED_EDGE('',*,*,#1391,.T.) ;
#2021 = ORIENTED_EDGE('',*,*,#1395,.T.) ;
#2022 = ORIENTED_EDGE('',*,*,#1398,.T.) ;
#2023 = ORIENTED_EDGE('',*,*,#1427,.F.) ;
#2024 = ORIENTED_EDGE('',*,*,#1435,.F.) ;
#2025 = ORIENTED_EDGE('',*,*,#1431,.T.) ;
#2026 = ORIENTED_EDGE('',*,*,#1436,.T.) ;
#2027 = ORIENTED_EDGE('',*,*,#1430,.F.) ;
#2028 = ORIENTED_EDGE('',*,*,#1437,.F.) ;
#2029 = ORIENTED_EDGE('',*,*,#1432,.T.) ;
#2030 = ORIENTED_EDGE('',*,*,#1435,.T.) ;
#2031 = ORIENTED_EDGE('',*,*,#1429,.F.) ;
#2032 = ORIENTED_EDGE('',*,*,#1438,.F.) ;
#2033 = ORIENTED_EDGE('',*,*,#1433,.T.) ;
#2034 = ORIENTED_EDGE('',*,*,#1437,.T.) ;
#2035 = ORIENTED_EDGE('',*,*,#1428,.F.) ;
#2036 = ORIENTED_EDGE('',*,*,#1436,.F.) ;
#2037 = ORIENTED_EDGE('',*,*,#1434,.T.) ;
#2038 = ORIENTED_EDGE('',*,*,#1438,.T.) ;
#2039 = PLANE('',#2338) ;
#2040 = PLANE('',#2339) ;
#2041 = PLANE('',#2340) ;
#2042 = PLANE('',#2341) ;
#2043 = PLANE('',#2342) ;
#2044 = PLANE('',#2343) ;
#2045 = PLANE('',#2344) ;
#2046 = PLANE('',#2345) ;
#2047 = PLANE('',#2346) ;
#2048 = PLANE('',#2347) ;
#2049 = PLANE('',#2352) ;
#2050 = PLANE('',#2361) ;
#2051 = PLANE('',#2362) ;
#2052 = PLANE('',#2363) ;
#2053 = PLANE('',#2364) ;
#2054 = PLANE('',#2365) ;
#2055 = PLANE('',#2366) ;
#2056 = PLANE('',#2367) ;
#2057 = PLANE('',#2368) ;
#2058 = PLANE('',#2370) ;
#2059 = PLANE('',#2371) ;
#2060 = PLANE('',#2372) ;
#2061 = PLANE('',#2373) ;
#2062 = PLANE('',#2374) ;
#2063 = PLANE('',#2375) ;
#2064 = PLANE('',#2376) ;
#2065 = PLANE('',#2377) ;
#2066 = PLANE('',#2378) ;
#2067 = PLANE('',#2379) ;
#2068 = PLANE('',#2384) ;
#2069 = PLANE('',#2393) ;
#2070 = PLANE('',#2394) ;
#2071 = PLANE('',#2395) ;
#2072 = PLANE('',#2396) ;
#2073 = PLANE('',#2397) ;
#2074 = PLANE('',#2398) ;
#2075 = PLANE('',#2399) ;
#2076 = PLANE('',#2400) ;
#2077 = PLANE('',#2402) ;
#2078 = PLANE('',#2403) ;
#2079 = PLANE('',#2404) ;
#2080 = PLANE('',#2405) ;
#2081 = PLANE('',#2406) ;
#2082 = PLANE('',#2407) ;
#2083 = PLANE('',#2408) ;
#2084 = PLANE('',#2409) ;
#2085 = PLANE('',#2410) ;
#2086 = PLANE('',#2411) ;
#2087 = PLANE('',#2416) ;
#2088 = PLANE('',#2425) ;
#2089 = PLANE('',#2426) ;
#2090 = PLANE('',#2427) ;
#2091 = PLANE('',#2428) ;
#2092 = PLANE('',#2430) ;
#2093 = PLANE('',#2431) ;
#2094 = PLANE('',#2432) ;
#2095 = PLANE('',#2433) ;
#2096 = PLANE('',#2434) ;
#2097 = PLANE('',#2435) ;
#2098 = PLANE('',#2436) ;
#2099 = PLANE('',#2437) ;
#2100 = PLANE('',#2438) ;
#2101 = PLANE('',#2439) ;
#2102 = PLANE('',#2444) ;
#2103 = PLANE('',#2454) ;
#2104 = PLANE('',#2455) ;
#2105 = PLANE('',#2456) ;
#2106 = PLANE('',#2457) ;
#2107 = PLANE('',#2458) ;
#2108 = PLANE('',#2459) ;
#2109 = PLANE('',#2460) ;
#2110 = PLANE('',#2461) ;
#2111 = PLANE('',#2462) ;
#2112 = PLANE('',#2463) ;
#2113 = PLANE('',#2464) ;
#2114 = PLANE('',#2465) ;
#2115 = PLANE('',#2466) ;
#2116 = PLANE('',#2467) ;
#2117 = PLANE('',#2468) ;
#2118 = PLANE('',#2469) ;
#2119 = PLANE('',#2470) ;
#2120 = PLANE('',#2471) ;
#2121 = PLANE('',#2472) ;
#2122 = PLANE('',#2473) ;
#2123 = PLANE('',#2475) ;
#2124 = PLANE('',#2476) ;
#2125 = PLANE('',#2477) ;
#2126 = PLANE('',#2478) ;
#2127 = PLANE('',#2479) ;
#2128 = PLANE('',#2480) ;
#2129 = PLANE('',#2481) ;
#2130 = PLANE('',#2482) ;
#2131 = PLANE('',#2483) ;
#2132 = PLANE('',#2484) ;
#2133 = PLANE('',#2485) ;
#2134 = PLANE('',#2486) ;
#2135 = PLANE('',#2487) ;
#2136 = PLANE('',#2488) ;
#2137 = PLANE('',#2489) ;
#2138 = PLANE('',#2490) ;
#2139 = PLANE('',#2491) ;
#2140 = PLANE('',#2492) ;
#2141 = PLANE('',#2493) ;
#2142 = PLANE('',#2494) ;
#2143 = ADVANCED_FACE('',(#141),#2039,.T.) ;
#2144 = ADVANCED_FACE('',(#142),#2040,.F.) ;
#2145 = ADVANCED_FACE('',(#143),#2041,.F.) ;
#2146 = ADVANCED_FACE('',(#144),#2042,.T.) ;
#2147 = ADVANCED_FACE('',(#145,#119,#120),#2043,.F.) ;
#2148 = ADVANCED_FACE('',(#146),#2044,.F.) ;
#2149 = ADVANCED_FACE('',(#147),#2045,.F.) ;
#2150 = ADVANCED_FACE('',(#148),#2046,.T.) ;
#2151 = ADVANCED_FACE('',(#149),#2047,.T.) ;
#2152 = ADVANCED_FACE('',(#150,#121),#2048,.T.) ;
#2153 = ADVANCED_FACE('',(#151,#122,#123),#2049,.T.) ;
#2154 = ADVANCED_FACE('',(#152),#71,.T.) ;
#2155 = ADVANCED_FACE('',(#153),#72,.T.) ;
#2156 = ADVANCED_FACE('',(#154),#73,.T.) ;
#2157 = ADVANCED_FACE('',(#155),#74,.T.) ;
#2158 = ADVANCED_FACE('',(#156),#2050,.F.) ;
#2159 = ADVANCED_FACE('',(#157),#2051,.F.) ;
#2160 = ADVANCED_FACE('',(#158),#2052,.F.) ;
#2161 = ADVANCED_FACE('',(#159),#2053,.F.) ;
#2162 = ADVANCED_FACE('',(#160),#2054,.F.) ;
#2163 = ADVANCED_FACE('',(#161),#2055,.F.) ;
#2164 = ADVANCED_FACE('',(#162),#2056,.F.) ;
#2165 = ADVANCED_FACE('',(#163),#2057,.F.) ;
#2166 = ADVANCED_FACE('',(#164),#2058,.T.) ;
#2167 = ADVANCED_FACE('',(#165),#2059,.F.) ;
#2168 = ADVANCED_FACE('',(#166),#2060,.F.) ;
#2169 = ADVANCED_FACE('',(#167),#2061,.T.) ;
#2170 = ADVANCED_FACE('',(#168,#124,#125),#2062,.F.) ;
#2171 = ADVANCED_FACE('',(#169),#2063,.F.) ;
#2172 = ADVANCED_FACE('',(#170),#2064,.F.) ;
#2173 = ADVANCED_FACE('',(#171),#2065,.T.) ;
#2174 = ADVANCED_FACE('',(#172),#2066,.T.) ;
#2175 = ADVANCED_FACE('',(#173,#126),#2067,.T.) ;
#2176 = ADVANCED_FACE('',(#174,#127,#128),#2068,.T.) ;
#2177 = ADVANCED_FACE('',(#175),#75,.T.) ;
#2178 = ADVANCED_FACE('',(#176),#76,.T.) ;
#2179 = ADVANCED_FACE('',(#177),#77,.T.) ;
#2180 = ADVANCED_FACE('',(#178),#78,.T.) ;
#2181 = ADVANCED_FACE('',(#179),#2069,.F.) ;
#2182 = ADVANCED_FACE('',(#180),#2070,.F.) ;
#2183 = ADVANCED_FACE('',(#181),#2071,.F.) ;
#2184 = ADVANCED_FACE('',(#182),#2072,.F.) ;
#2185 = ADVANCED_FACE('',(#183),#2073,.F.) ;
#2186 = ADVANCED_FACE('',(#184),#2074,.F.) ;
#2187 = ADVANCED_FACE('',(#185),#2075,.F.) ;
#2188 = ADVANCED_FACE('',(#186),#2076,.F.) ;
#2189 = ADVANCED_FACE('',(#187),#2077,.T.) ;
#2190 = ADVANCED_FACE('',(#188),#2078,.F.) ;
#2191 = ADVANCED_FACE('',(#189),#2079,.F.) ;
#2192 = ADVANCED_FACE('',(#190),#2080,.T.) ;
#2193 = ADVANCED_FACE('',(#191,#129),#2081,.F.) ;
#2194 = ADVANCED_FACE('',(#192),#2082,.F.) ;
#2195 = ADVANCED_FACE('',(#193),#2083,.F.) ;
#2196 = ADVANCED_FACE('',(#194),#2084,.T.) ;
#2197 = ADVANCED_FACE('',(#195),#2085,.T.) ;
#2198 = ADVANCED_FACE('',(#196,#130),#2086,.T.) ;
#2199 = ADVANCED_FACE('',(#197,#131),#2087,.T.) ;
#2200 = ADVANCED_FACE('',(#198),#79,.T.) ;
#2201 = ADVANCED_FACE('',(#199),#80,.T.) ;
#2202 = ADVANCED_FACE('',(#200),#81,.T.) ;
#2203 = ADVANCED_FACE('',(#201),#82,.T.) ;
#2204 = ADVANCED_FACE('',(#202),#2088,.F.) ;
#2205 = ADVANCED_FACE('',(#203),#2089,.F.) ;
#2206 = ADVANCED_FACE('',(#204),#2090,.F.) ;
#2207 = ADVANCED_FACE('',(#205),#2091,.F.) ;
#2208 = ADVANCED_FACE('',(#206),#2092,.T.) ;
#2209 = ADVANCED_FACE('',(#207),#2093,.F.) ;
#2210 = ADVANCED_FACE('',(#208),#2094,.F.) ;
#2211 = ADVANCED_FACE('',(#209),#2095,.T.) ;
#2212 = ADVANCED_FACE('',(#210),#2096,.F.) ;
#2213 = ADVANCED_FACE('',(#211),#2097,.F.) ;
#2214 = ADVANCED_FACE('',(#212),#2098,.F.) ;
#2215 = ADVANCED_FACE('',(#213),#2099,.T.) ;
#2216 = ADVANCED_FACE('',(#214),#2100,.T.) ;
#2217 = ADVANCED_FACE('',(#215,#132),#2101,.T.) ;
#2218 = ADVANCED_FACE('',(#216),#2102,.T.) ;
#2219 = ADVANCED_FACE('',(#217),#83,.T.) ;
#2220 = ADVANCED_FACE('',(#218),#84,.T.) ;
#2221 = ADVANCED_FACE('',(#219),#85,.T.) ;
#2222 = ADVANCED_FACE('',(#220),#86,.T.) ;
#2223 = ADVANCED_FACE('',(#221),#2103,.F.) ;
#2224 = ADVANCED_FACE('',(#222),#2104,.F.) ;
#2225 = ADVANCED_FACE('',(#223),#2105,.F.) ;
#2226 = ADVANCED_FACE('',(#224),#2106,.F.) ;
#2227 = ADVANCED_FACE('',(#225,#133),#2107,.T.) ;
#2228 = ADVANCED_FACE('',(#226,#134),#2108,.F.) ;
#2229 = ADVANCED_FACE('',(#227),#2109,.F.) ;
#2230 = ADVANCED_FACE('',(#228),#2110,.F.) ;
#2231 = ADVANCED_FACE('',(#229),#2111,.F.) ;
#2232 = ADVANCED_FACE('',(#230),#2112,.F.) ;
#2233 = ADVANCED_FACE('',(#231),#2113,.T.) ;
#2234 = ADVANCED_FACE('',(#232),#2114,.T.) ;
#2235 = ADVANCED_FACE('',(#233),#2115,.T.) ;
#2236 = ADVANCED_FACE('',(#234),#2116,.T.) ;
#2237 = ADVANCED_FACE('',(#235,#135),#2117,.T.) ;
#2238 = ADVANCED_FACE('',(#236,#136),#2118,.F.) ;
#2239 = ADVANCED_FACE('',(#237),#2119,.T.) ;
#2240 = ADVANCED_FACE('',(#238),#2120,.T.) ;
#2241 = ADVANCED_FACE('',(#239),#2121,.T.) ;
#2242 = ADVANCED_FACE('',(#240),#2122,.T.) ;
#2243 = ADVANCED_FACE('',(#241),#2123,.F.) ;
#2244 = ADVANCED_FACE('',(#242),#2124,.F.) ;
#2245 = ADVANCED_FACE('',(#243),#2125,.F.) ;
#2246 = ADVANCED_FACE('',(#244),#2126,.F.) ;
#2247 = ADVANCED_FACE('',(#245,#137),#2127,.T.) ;
#2248 = ADVANCED_FACE('',(#246,#138),#2128,.F.) ;
#2249 = ADVANCED_FACE('',(#247),#2129,.F.) ;
#2250 = ADVANCED_FACE('',(#248),#2130,.F.) ;
#2251 = ADVANCED_FACE('',(#249),#2131,.F.) ;
#2252 = ADVANCED_FACE('',(#250),#2132,.F.) ;
#2253 = ADVANCED_FACE('',(#251),#2133,.T.) ;
#2254 = ADVANCED_FACE('',(#252),#2134,.T.) ;
#2255 = ADVANCED_FACE('',(#253),#2135,.T.) ;
#2256 = ADVANCED_FACE('',(#254),#2136,.T.) ;
#2257 = ADVANCED_FACE('',(#255,#139),#2137,.T.) ;
#2258 = ADVANCED_FACE('',(#256,#140),#2138,.F.) ;
#2259 = ADVANCED_FACE('',(#257),#2139,.T.) ;
#2260 = ADVANCED_FACE('',(#258),#2140,.T.) ;
#2261 = ADVANCED_FACE('',(#259),#2141,.T.) ;
#2262 = ADVANCED_FACE('',(#260),#2142,.T.) ;
#2263 = CLOSED_SHELL('',(#2143,#2144,#2145,#2146,#2147,#2148,#2149,#2150,
#2151,#2152,#2153,#2154,#2155,#2156,#2157,#2158,#2159,#2160,#2161,#2162,
#2163,#2164,#2165)) ;
#2264 = CLOSED_SHELL('',(#2166,#2167,#2168,#2169,#2170,#2171,#2172,#2173,
#2174,#2175,#2176,#2177,#2178,#2179,#2180,#2181,#2182,#2183,#2184,#2185,
#2186,#2187,#2188)) ;
#2265 = CLOSED_SHELL('',(#2189,#2190,#2191,#2192,#2193,#2194,#2195,#2196,
#2197,#2198,#2199,#2200,#2201,#2202,#2203,#2204,#2205,#2206,#2207)) ;
#2266 = CLOSED_SHELL('',(#2208,#2209,#2210,#2211,#2212,#2213,#2214,#2215,
#2216,#2217,#2218,#2219,#2220,#2221,#2222)) ;
#2267 = CLOSED_SHELL('',(#2223,#2224,#2225,#2226,#2227,#2228,#2229,#2230,
#2231,#2232,#2233,#2234,#2235,#2236,#2237,#2238,#2239,#2240,#2241,#2242)) ;
#2268 = CLOSED_SHELL('',(#2243,#2244,#2245,#2246,#2247,#2248,#2249,#2250,
#2251,#2252,#2253,#2254,#2255,#2256,#2257,#2258,#2259,#2260,#2261,#2262)) ;
#2269 = DERIVED_UNIT_ELEMENT(#2281,1.) ;
#2270 = DERIVED_UNIT_ELEMENT(#3761,-3.) ;
#2271 = DERIVED_UNIT_ELEMENT(#2281,1.) ;
#2272 = DERIVED_UNIT_ELEMENT(#3761,-3.) ;
#2273 = DERIVED_UNIT_ELEMENT(#2281,1.) ;
#2274 = DERIVED_UNIT_ELEMENT(#3761,-3.) ;
#2275 = DERIVED_UNIT_ELEMENT(#2281,1.) ;
#2276 = DERIVED_UNIT_ELEMENT(#3761,-3.) ;
#2277 = DERIVED_UNIT_ELEMENT(#2281,1.) ;
#2278 = DERIVED_UNIT_ELEMENT(#3761,-3.) ;
#2279 = DERIVED_UNIT_ELEMENT(#2281,1.) ;
#2280 = DERIVED_UNIT_ELEMENT(#3761,-3.) ;
#2281 = (
MASS_UNIT()
NAMED_UNIT(*)
SI_UNIT(.KILO.,.GRAM.)
) ;
#2282 = DERIVED_UNIT((#2269,#2270)) ;
#2283 = DERIVED_UNIT((#2271,#2272)) ;
#2284 = DERIVED_UNIT((#2273,#2274)) ;
#2285 = DERIVED_UNIT((#2275,#2276)) ;
#2286 = DERIVED_UNIT((#2277,#2278)) ;
#2287 = DERIVED_UNIT((#2279,#2280)) ;
#2288 = MEASURE_REPRESENTATION_ITEM('density measure',
POSITIVE_RATIO_MEASURE(7850.),#2282) ;
#2289 = MEASURE_REPRESENTATION_ITEM('density measure',
POSITIVE_RATIO_MEASURE(7850.),#2283) ;
#2290 = MEASURE_REPRESENTATION_ITEM('density measure',
POSITIVE_RATIO_MEASURE(7850.),#2284) ;
#2291 = MEASURE_REPRESENTATION_ITEM('density measure',
POSITIVE_RATIO_MEASURE(7850.),#2285) ;
#2292 = MEASURE_REPRESENTATION_ITEM('density measure',
POSITIVE_RATIO_MEASURE(7850.),#2286) ;
#2293 = MEASURE_REPRESENTATION_ITEM('density measure',
POSITIVE_RATIO_MEASURE(7850.),#2287) ;
#2294 = PROPERTY_DEFINITION_REPRESENTATION(#2324,#2306) ;
#2295 = PROPERTY_DEFINITION_REPRESENTATION(#2325,#2307) ;
#2296 = PROPERTY_DEFINITION_REPRESENTATION(#2326,#2308) ;
#2297 = PROPERTY_DEFINITION_REPRESENTATION(#2327,#2309) ;
#2298 = PROPERTY_DEFINITION_REPRESENTATION(#2328,#2310) ;
#2299 = PROPERTY_DEFINITION_REPRESENTATION(#2329,#2311) ;
#2300 = PROPERTY_DEFINITION_REPRESENTATION(#2330,#2312) ;
#2301 = PROPERTY_DEFINITION_REPRESENTATION(#2331,#2313) ;
#2302 = PROPERTY_DEFINITION_REPRESENTATION(#2332,#2314) ;
#2303 = PROPERTY_DEFINITION_REPRESENTATION(#2333,#2315) ;
#2304 = PROPERTY_DEFINITION_REPRESENTATION(#2334,#2316) ;
#2305 = PROPERTY_DEFINITION_REPRESENTATION(#2335,#2317) ;
#2306 = REPRESENTATION('material name',(#2318),#3753) ;
#2307 = REPRESENTATION('density',(#2288),#3753) ;
#2308 = REPRESENTATION('material name',(#2319),#3754) ;
#2309 = REPRESENTATION('density',(#2289),#3754) ;
#2310 = REPRESENTATION('material name',(#2320),#3755) ;
#2311 = REPRESENTATION('density',(#2290),#3755) ;
#2312 = REPRESENTATION('material name',(#2321),#3756) ;
#2313 = REPRESENTATION('density',(#2291),#3756) ;
#2314 = REPRESENTATION('material name',(#2322),#3757) ;
#2315 = REPRESENTATION('density',(#2292),#3757) ;
#2316 = REPRESENTATION('material name',(#2323),#3758) ;
#2317 = REPRESENTATION('density',(#2293),#3758) ;
#2318 = DESCRIPTIVE_REPRESENTATION_ITEM('Steel','Steel') ;
#2319 = DESCRIPTIVE_REPRESENTATION_ITEM('Steel','Steel') ;
#2320 = DESCRIPTIVE_REPRESENTATION_ITEM('Steel','Steel') ;
#2321 = DESCRIPTIVE_REPRESENTATION_ITEM('Steel','Steel') ;
#2322 = DESCRIPTIVE_REPRESENTATION_ITEM('Steel','Steel') ;
#2323 = DESCRIPTIVE_REPRESENTATION_ITEM('Steel','Steel') ;
#2324 = PROPERTY_DEFINITION('material property','material name',#3796) ;
#2325 = PROPERTY_DEFINITION('material property','density of part',#3796) ;
#2326 = PROPERTY_DEFINITION('material property','material name',#3797) ;
#2327 = PROPERTY_DEFINITION('material property','density of part',#3797) ;
#2328 = PROPERTY_DEFINITION('material property','material name',#3798) ;
#2329 = PROPERTY_DEFINITION('material property','density of part',#3798) ;
#2330 = PROPERTY_DEFINITION('material property','material name',#3799) ;
#2331 = PROPERTY_DEFINITION('material property','density of part',#3799) ;
#2332 = PROPERTY_DEFINITION('material property','material name',#3800) ;
#2333 = PROPERTY_DEFINITION('material property','density of part',#3800) ;
#2334 = PROPERTY_DEFINITION('material property','material name',#3801) ;
#2335 = PROPERTY_DEFINITION('material property','density of part',#3801) ;
#2336 = AXIS2_PLACEMENT_3D('',#3108,#2504,#2505) ;
#2337 = AXIS2_PLACEMENT_3D('',#3109,#2506,#2507) ;
#2338 = AXIS2_PLACEMENT_3D('',#3110,#2508,#2509) ;
#2339 = AXIS2_PLACEMENT_3D('',#3119,#2514,#2515) ;
#2340 = AXIS2_PLACEMENT_3D('',#3125,#2519,#2520) ;
#2341 = AXIS2_PLACEMENT_3D('',#3131,#2524,#2525) ;
#2342 = AXIS2_PLACEMENT_3D('',#3134,#2528,#2529) ;
#2343 = AXIS2_PLACEMENT_3D('',#3151,#2538,#2539) ;
#2344 = AXIS2_PLACEMENT_3D('',#3160,#2544,#2545) ;
#2345 = AXIS2_PLACEMENT_3D('',#3169,#2550,#2551) ;
#2346 = AXIS2_PLACEMENT_3D('',#3178,#2556,#2557) ;
#2347 = AXIS2_PLACEMENT_3D('',#3187,#2562,#2563) ;
#2348 = AXIS2_PLACEMENT_3D('',#3188,#2564,#2565) ;
#2349 = AXIS2_PLACEMENT_3D('',#3189,#2566,#2567) ;
#2350 = AXIS2_PLACEMENT_3D('',#3190,#2568,#2569) ;
#2351 = AXIS2_PLACEMENT_3D('',#3191,#2570,#2571) ;
#2352 = AXIS2_PLACEMENT_3D('',#3192,#2572,#2573) ;
#2353 = AXIS2_PLACEMENT_3D('',#3193,#2574,#2575) ;
#2354 = AXIS2_PLACEMENT_3D('',#3194,#2576,#2577) ;
#2355 = AXIS2_PLACEMENT_3D('',#3195,#2578,#2579) ;
#2356 = AXIS2_PLACEMENT_3D('',#3196,#2580,#2581) ;
#2357 = AXIS2_PLACEMENT_3D('',#3213,#2590,#2591) ;
#2358 = AXIS2_PLACEMENT_3D('',#3214,#2592,#2593) ;
#2359 = AXIS2_PLACEMENT_3D('',#3215,#2594,#2595) ;
#2360 = AXIS2_PLACEMENT_3D('',#3216,#2596,#2597) ;
#2361 = AXIS2_PLACEMENT_3D('',#3217,#2598,#2599) ;
#2362 = AXIS2_PLACEMENT_3D('',#3220,#2602,#2603) ;
#2363 = AXIS2_PLACEMENT_3D('',#3222,#2605,#2606) ;
#2364 = AXIS2_PLACEMENT_3D('',#3224,#2608,#2609) ;
#2365 = AXIS2_PLACEMENT_3D('',#3225,#2610,#2611) ;
#2366 = AXIS2_PLACEMENT_3D('',#3228,#2614,#2615) ;
#2367 = AXIS2_PLACEMENT_3D('',#3230,#2617,#2618) ;
#2368 = AXIS2_PLACEMENT_3D('',#3232,#2620,#2621) ;
#2369 = AXIS2_PLACEMENT_3D('',#3233,#2622,#2623) ;
#2370 = AXIS2_PLACEMENT_3D('',#3234,#2624,#2625) ;
#2371 = AXIS2_PLACEMENT_3D('',#3243,#2630,#2631) ;
#2372 = AXIS2_PLACEMENT_3D('',#3249,#2635,#2636) ;
#2373 = AXIS2_PLACEMENT_3D('',#3255,#2640,#2641) ;
#2374 = AXIS2_PLACEMENT_3D('',#3258,#2644,#2645) ;
#2375 = AXIS2_PLACEMENT_3D('',#3275,#2654,#2655) ;
#2376 = AXIS2_PLACEMENT_3D('',#3284,#2660,#2661) ;
#2377 = AXIS2_PLACEMENT_3D('',#3293,#2666,#2667) ;
#2378 = AXIS2_PLACEMENT_3D('',#3302,#2672,#2673) ;
#2379 = AXIS2_PLACEMENT_3D('',#3311,#2678,#2679) ;
#2380 = AXIS2_PLACEMENT_3D('',#3312,#2680,#2681) ;
#2381 = AXIS2_PLACEMENT_3D('',#3313,#2682,#2683) ;
#2382 = AXIS2_PLACEMENT_3D('',#3314,#2684,#2685) ;
#2383 = AXIS2_PLACEMENT_3D('',#3315,#2686,#2687) ;
#2384 = AXIS2_PLACEMENT_3D('',#3316,#2688,#2689) ;
#2385 = AXIS2_PLACEMENT_3D('',#3317,#2690,#2691) ;
#2386 = AXIS2_PLACEMENT_3D('',#3318,#2692,#2693) ;
#2387 = AXIS2_PLACEMENT_3D('',#3319,#2694,#2695) ;
#2388 = AXIS2_PLACEMENT_3D('',#3320,#2696,#2697) ;
#2389 = AXIS2_PLACEMENT_3D('',#3337,#2706,#2707) ;
#2390 = AXIS2_PLACEMENT_3D('',#3338,#2708,#2709) ;
#2391 = AXIS2_PLACEMENT_3D('',#3339,#2710,#2711) ;
#2392 = AXIS2_PLACEMENT_3D('',#3340,#2712,#2713) ;
#2393 = AXIS2_PLACEMENT_3D('',#3341,#2714,#2715) ;
#2394 = AXIS2_PLACEMENT_3D('',#3344,#2718,#2719) ;
#2395 = AXIS2_PLACEMENT_3D('',#3346,#2721,#2722) ;
#2396 = AXIS2_PLACEMENT_3D('',#3348,#2724,#2725) ;
#2397 = AXIS2_PLACEMENT_3D('',#3349,#2726,#2727) ;
#2398 = AXIS2_PLACEMENT_3D('',#3352,#2730,#2731) ;
#2399 = AXIS2_PLACEMENT_3D('',#3354,#2733,#2734) ;
#2400 = AXIS2_PLACEMENT_3D('',#3356,#2736,#2737) ;
#2401 = AXIS2_PLACEMENT_3D('',#3357,#2738,#2739) ;
#2402 = AXIS2_PLACEMENT_3D('',#3358,#2740,#2741) ;
#2403 = AXIS2_PLACEMENT_3D('',#3367,#2746,#2747) ;
#2404 = AXIS2_PLACEMENT_3D('',#3373,#2751,#2752) ;
#2405 = AXIS2_PLACEMENT_3D('',#3379,#2756,#2757) ;
#2406 = AXIS2_PLACEMENT_3D('',#3382,#2760,#2761) ;
#2407 = AXIS2_PLACEMENT_3D('',#3391,#2766,#2767) ;
#2408 = AXIS2_PLACEMENT_3D('',#3400,#2772,#2773) ;
#2409 = AXIS2_PLACEMENT_3D('',#3409,#2778,#2779) ;
#2410 = AXIS2_PLACEMENT_3D('',#3418,#2784,#2785) ;
#2411 = AXIS2_PLACEMENT_3D('',#3427,#2790,#2791) ;
#2412 = AXIS2_PLACEMENT_3D('',#3428,#2792,#2793) ;
#2413 = AXIS2_PLACEMENT_3D('',#3429,#2794,#2795) ;
#2414 = AXIS2_PLACEMENT_3D('',#3430,#2796,#2797) ;
#2415 = AXIS2_PLACEMENT_3D('',#3431,#2798,#2799) ;
#2416 = AXIS2_PLACEMENT_3D('',#3432,#2800,#2801) ;
#2417 = AXIS2_PLACEMENT_3D('',#3433,#2802,#2803) ;
#2418 = AXIS2_PLACEMENT_3D('',#3434,#2804,#2805) ;
#2419 = AXIS2_PLACEMENT_3D('',#3435,#2806,#2807) ;
#2420 = AXIS2_PLACEMENT_3D('',#3436,#2808,#2809) ;
#2421 = AXIS2_PLACEMENT_3D('',#3445,#2814,#2815) ;
#2422 = AXIS2_PLACEMENT_3D('',#3446,#2816,#2817) ;
#2423 = AXIS2_PLACEMENT_3D('',#3447,#2818,#2819) ;
#2424 = AXIS2_PLACEMENT_3D('',#3448,#2820,#2821) ;
#2425 = AXIS2_PLACEMENT_3D('',#3449,#2822,#2823) ;
#2426 = AXIS2_PLACEMENT_3D('',#3452,#2826,#2827) ;
#2427 = AXIS2_PLACEMENT_3D('',#3454,#2829,#2830) ;
#2428 = AXIS2_PLACEMENT_3D('',#3456,#2832,#2833) ;
#2429 = AXIS2_PLACEMENT_3D('',#3457,#2834,#2835) ;
#2430 = AXIS2_PLACEMENT_3D('',#3458,#2836,#2837) ;
#2431 = AXIS2_PLACEMENT_3D('',#3467,#2842,#2843) ;
#2432 = AXIS2_PLACEMENT_3D('',#3473,#2847,#2848) ;
#2433 = AXIS2_PLACEMENT_3D('',#3479,#2852,#2853) ;
#2434 = AXIS2_PLACEMENT_3D('',#3482,#2856,#2857) ;
#2435 = AXIS2_PLACEMENT_3D('',#3483,#2858,#2859) ;
#2436 = AXIS2_PLACEMENT_3D('',#3492,#2864,#2865) ;
#2437 = AXIS2_PLACEMENT_3D('',#3501,#2870,#2871) ;
#2438 = AXIS2_PLACEMENT_3D('',#3510,#2876,#2877) ;
#2439 = AXIS2_PLACEMENT_3D('',#3519,#2882,#2883) ;
#2440 = AXIS2_PLACEMENT_3D('',#3520,#2884,#2885) ;
#2441 = AXIS2_PLACEMENT_3D('',#3521,#2886,#2887) ;
#2442 = AXIS2_PLACEMENT_3D('',#3522,#2888,#2889) ;
#2443 = AXIS2_PLACEMENT_3D('',#3523,#2890,#2891) ;
#2444 = AXIS2_PLACEMENT_3D('',#3524,#2892,#2893) ;
#2445 = AXIS2_PLACEMENT_3D('',#3525,#2894,#2895) ;
#2446 = AXIS2_PLACEMENT_3D('',#3526,#2896,#2897) ;
#2447 = AXIS2_PLACEMENT_3D('',#3527,#2898,#2899) ;
#2448 = AXIS2_PLACEMENT_3D('',#3528,#2900,#2901) ;
#2449 = AXIS2_PLACEMENT_3D('',#3529,#2902,#2903) ;
#2450 = AXIS2_PLACEMENT_3D('',#3530,#2904,#2905) ;
#2451 = AXIS2_PLACEMENT_3D('',#3531,#2906,#2907) ;
#2452 = AXIS2_PLACEMENT_3D('',#3532,#2908,#2909) ;
#2453 = AXIS2_PLACEMENT_3D('',#3533,#2910,#2911) ;
#2454 = AXIS2_PLACEMENT_3D('',#3534,#2912,#2913) ;
#2455 = AXIS2_PLACEMENT_3D('',#3543,#2918,#2919) ;
#2456 = AXIS2_PLACEMENT_3D('',#3549,#2923,#2924) ;
#2457 = AXIS2_PLACEMENT_3D('',#3555,#2928,#2929) ;
#2458 = AXIS2_PLACEMENT_3D('',#3558,#2932,#2933) ;
#2459 = AXIS2_PLACEMENT_3D('',#3567,#2938,#2939) ;
#2460 = AXIS2_PLACEMENT_3D('',#3584,#2948,#2949) ;
#2461 = AXIS2_PLACEMENT_3D('',#3587,#2952,#2953) ;
#2462 = AXIS2_PLACEMENT_3D('',#3589,#2955,#2956) ;
#2463 = AXIS2_PLACEMENT_3D('',#3591,#2958,#2959) ;
#2464 = AXIS2_PLACEMENT_3D('',#3592,#2960,#2961) ;
#2465 = AXIS2_PLACEMENT_3D('',#3598,#2965,#2966) ;
#2466 = AXIS2_PLACEMENT_3D('',#3602,#2969,#2970) ;
#2467 = AXIS2_PLACEMENT_3D('',#3606,#2973,#2974) ;
#2468 = AXIS2_PLACEMENT_3D('',#3608,#2976,#2977) ;
#2469 = AXIS2_PLACEMENT_3D('',#3617,#2982,#2983) ;
#2470 = AXIS2_PLACEMENT_3D('',#3626,#2988,#2989) ;
#2471 = AXIS2_PLACEMENT_3D('',#3629,#2992,#2993) ;
#2472 = AXIS2_PLACEMENT_3D('',#3631,#2995,#2996) ;
#2473 = AXIS2_PLACEMENT_3D('',#3633,#2998,#2999) ;
#2474 = AXIS2_PLACEMENT_3D('',#3634,#3000,#3001) ;
#2475 = AXIS2_PLACEMENT_3D('',#3635,#3002,#3003) ;
#2476 = AXIS2_PLACEMENT_3D('',#3644,#3008,#3009) ;
#2477 = AXIS2_PLACEMENT_3D('',#3650,#3013,#3014) ;
#2478 = AXIS2_PLACEMENT_3D('',#3656,#3018,#3019) ;
#2479 = AXIS2_PLACEMENT_3D('',#3659,#3022,#3023) ;
#2480 = AXIS2_PLACEMENT_3D('',#3668,#3028,#3029) ;
#2481 = AXIS2_PLACEMENT_3D('',#3685,#3038,#3039) ;
#2482 = AXIS2_PLACEMENT_3D('',#3688,#3042,#3043) ;
#2483 = AXIS2_PLACEMENT_3D('',#3690,#3045,#3046) ;
#2484 = AXIS2_PLACEMENT_3D('',#3692,#3048,#3049) ;
#2485 = AXIS2_PLACEMENT_3D('',#3693,#3050,#3051) ;
#2486 = AXIS2_PLACEMENT_3D('',#3699,#3055,#3056) ;
#2487 = AXIS2_PLACEMENT_3D('',#3703,#3059,#3060) ;
#2488 = AXIS2_PLACEMENT_3D('',#3707,#3063,#3064) ;
#2489 = AXIS2_PLACEMENT_3D('',#3709,#3066,#3067) ;
#2490 = AXIS2_PLACEMENT_3D('',#3718,#3072,#3073) ;
#2491 = AXIS2_PLACEMENT_3D('',#3727,#3078,#3079) ;
#2492 = AXIS2_PLACEMENT_3D('',#3730,#3082,#3083) ;
#2493 = AXIS2_PLACEMENT_3D('',#3732,#3085,#3086) ;
#2494 = AXIS2_PLACEMENT_3D('',#3734,#3088,#3089) ;
#2495 = AXIS2_PLACEMENT_3D('',#3735,#3090,#3091) ;
#2496 = AXIS2_PLACEMENT_3D('',#3736,#3092,#3093) ;
#2497 = AXIS2_PLACEMENT_3D('',#3737,#3094,#3095) ;
#2498 = AXIS2_PLACEMENT_3D('',#3738,#3096,#3097) ;
#2499 = AXIS2_PLACEMENT_3D('',#3739,#3098,#3099) ;
#2500 = AXIS2_PLACEMENT_3D('',#3740,#3100,#3101) ;
#2501 = AXIS2_PLACEMENT_3D('',#3741,#3102,#3103) ;
#2502 = AXIS2_PLACEMENT_3D('',#3742,#3104,#3105) ;
#2503 = AXIS2_PLACEMENT_3D('',#3743,#3106,#3107) ;
#2504 = DIRECTION('axis',(0.,0.,1.)) ;
#2505 = DIRECTION('refdir',(1.,0.,0.)) ;
#2506 = DIRECTION('axis',(0.,0.,1.)) ;
#2507 = DIRECTION('refdir',(1.,0.,0.)) ;
#2508 = DIRECTION('center_axis',(1.28102656687518E-16,-1.,0.)) ;
#2509 = DIRECTION('ref_axis',(1.,1.28102656687518E-16,0.)) ;
#2510 = DIRECTION('',(-1.,-1.28102656687518E-16,0.)) ;
#2511 = DIRECTION('',(0.,0.,-1.)) ;
#2512 = DIRECTION('',(-1.,-1.28102656687518E-16,0.)) ;
#2513 = DIRECTION('',(0.,0.,-1.)) ;
#2514 = DIRECTION('center_axis',(-1.,0.,0.)) ;
#2515 = DIRECTION('ref_axis',(0.,0.,1.)) ;
#2516 = DIRECTION('',(0.,1.,0.)) ;
#2517 = DIRECTION('',(0.,0.,-1.)) ;
#2518 = DIRECTION('',(0.,1.,0.)) ;
#2519 = DIRECTION('center_axis',(8.5401771125012E-17,-1.,0.)) ;
#2520 = DIRECTION('ref_axis',(1.,8.5401771125012E-17,0.)) ;
#2521 = DIRECTION('',(-1.,-8.54017711250121E-17,0.)) ;
#2522 = DIRECTION('',(0.,0.,-1.)) ;
#2523 = DIRECTION('',(-1.,-8.5401771125012E-17,0.)) ;
#2524 = DIRECTION('center_axis',(-1.,0.,0.)) ;
#2525 = DIRECTION('ref_axis',(0.,0.,1.)) ;
#2526 = DIRECTION('',(0.,1.,0.)) ;
#2527 = DIRECTION('',(0.,1.,0.)) ;
#2528 = DIRECTION('center_axis',(0.,0.,-1.)) ;
#2529 = DIRECTION('ref_axis',(-1.,0.,0.)) ;
#2530 = DIRECTION('',(1.,0.,0.)) ;
#2531 = DIRECTION('',(0.,-1.,0.)) ;
#2532 = DIRECTION('',(-1.,7.43452918275775E-17,0.)) ;
#2533 = DIRECTION('',(0.,1.,0.)) ;
#2534 = DIRECTION('',(1.,-1.18952466924124E-16,0.)) ;
#2535 = DIRECTION('',(0.,-1.,0.)) ;
#2536 = DIRECTION('',(-1.,0.,0.)) ;
#2537 = DIRECTION('',(0.,1.,0.)) ;
#2538 = DIRECTION('center_axis',(-1.,0.,0.)) ;
#2539 = DIRECTION('ref_axis',(0.,0.,1.)) ;
#2540 = DIRECTION('',(0.,1.,0.)) ;
#2541 = DIRECTION('',(0.,0.,-1.)) ;
#2542 = DIRECTION('',(0.,1.,0.)) ;
#2543 = DIRECTION('',(0.,0.,1.)) ;
#2544 = DIRECTION('center_axis',(7.95288699588221E-17,-1.,0.)) ;
#2545 = DIRECTION('ref_axis',(1.,7.95288699588221E-17,0.)) ;
#2546 = DIRECTION('',(-1.,-7.95288699588221E-17,0.)) ;
#2547 = DIRECTION('',(0.,0.,1.)) ;
#2548 = DIRECTION('',(-1.,-7.95288699588221E-17,0.)) ;
#2549 = DIRECTION('',(0.,0.,-1.)) ;
#2550 = DIRECTION('center_axis',(-1.,0.,0.)) ;
#2551 = DIRECTION('ref_axis',(0.,0.,1.)) ;
#2552 = DIRECTION('',(0.,1.,0.)) ;
#2553 = DIRECTION('',(0.,0.,1.)) ;
#2554 = DIRECTION('',(0.,1.,0.)) ;
#2555 = DIRECTION('',(0.,0.,-1.)) ;
#2556 = DIRECTION('center_axis',(1.19293304938233E-16,-1.,0.)) ;
#2557 = DIRECTION('ref_axis',(1.,1.19293304938233E-16,0.)) ;
#2558 = DIRECTION('',(-1.,-1.19293304938233E-16,0.)) ;
#2559 = DIRECTION('',(0.,0.,1.)) ;
#2560 = DIRECTION('',(-1.,-1.19293304938233E-16,0.)) ;
#2561 = DIRECTION('',(0.,0.,-1.)) ;
#2562 = DIRECTION('center_axis',(0.,0.,1.)) ;
#2563 = DIRECTION('ref_axis',(1.,0.,0.)) ;
#2564 = DIRECTION('center_axis',(0.,0.,1.)) ;
#2565 = DIRECTION('ref_axis',(1.,0.,0.)) ;
#2566 = DIRECTION('center_axis',(0.,0.,1.)) ;
#2567 = DIRECTION('ref_axis',(1.,0.,0.)) ;
#2568 = DIRECTION('center_axis',(0.,0.,1.)) ;
#2569 = DIRECTION('ref_axis',(1.,0.,0.)) ;
#2570 = DIRECTION('center_axis',(0.,0.,1.)) ;
#2571 = DIRECTION('ref_axis',(1.,0.,0.)) ;
#2572 = DIRECTION('center_axis',(0.,0.,-1.)) ;
#2573 = DIRECTION('ref_axis',(-1.,0.,0.)) ;
#2574 = DIRECTION('center_axis',(0.,0.,-1.)) ;
#2575 = DIRECTION('ref_axis',(-1.,0.,0.)) ;
#2576 = DIRECTION('center_axis',(0.,0.,-1.)) ;
#2577 = DIRECTION('ref_axis',(-1.,0.,0.)) ;
#2578 = DIRECTION('center_axis',(0.,0.,-1.)) ;
#2579 = DIRECTION('ref_axis',(-1.,0.,0.)) ;
#2580 = DIRECTION('center_axis',(0.,0.,-1.)) ;
#2581 = DIRECTION('ref_axis',(-1.,0.,0.)) ;
#2582 = DIRECTION('',(0.,-1.,0.)) ;
#2583 = DIRECTION('',(1.,0.,0.)) ;
#2584 = DIRECTION('',(0.,1.,0.)) ;
#2585 = DIRECTION('',(-1.,7.43452918275774E-17,0.)) ;
#2586 = DIRECTION('',(0.,-1.,0.)) ;
#2587 = DIRECTION('',(1.,-1.18952466924124E-16,0.)) ;
#2588 = DIRECTION('',(0.,1.,0.)) ;
#2589 = DIRECTION('',(-1.,0.,0.)) ;
#2590 = DIRECTION('center_axis',(0.,0.,1.)) ;
#2591 = DIRECTION('ref_axis',(1.,0.,0.)) ;
#2592 = DIRECTION('center_axis',(0.,0.,-1.)) ;
#2593 = DIRECTION('ref_axis',(-1.,0.,0.)) ;
#2594 = DIRECTION('center_axis',(0.,0.,1.)) ;
#2595 = DIRECTION('ref_axis',(1.,0.,0.)) ;
#2596 = DIRECTION('center_axis',(0.,0.,-1.)) ;
#2597 = DIRECTION('ref_axis',(-1.,0.,0.)) ;
#2598 = DIRECTION('center_axis',(1.,0.,0.)) ;
#2599 = DIRECTION('ref_axis',(0.,0.,-1.)) ;
#2600 = DIRECTION('',(0.,0.,-1.)) ;
#2601 = DIRECTION('',(0.,0.,-1.)) ;
#2602 = DIRECTION('center_axis',(1.18952466924124E-16,1.,0.)) ;
#2603 = DIRECTION('ref_axis',(-1.,1.18952466924124E-16,0.)) ;
#2604 = DIRECTION('',(0.,0.,-1.)) ;
#2605 = DIRECTION('center_axis',(-1.,0.,0.)) ;
#2606 = DIRECTION('ref_axis',(0.,0.,1.)) ;
#2607 = DIRECTION('',(0.,0.,-1.)) ;
#2608 = DIRECTION('center_axis',(0.,-1.,0.)) ;
#2609 = DIRECTION('ref_axis',(0.,0.,-1.)) ;
#2610 = DIRECTION('center_axis',(1.,0.,0.)) ;
#2611 = DIRECTION('ref_axis',(0.,0.,-1.)) ;
#2612 = DIRECTION('',(0.,0.,-1.)) ;
#2613 = DIRECTION('',(0.,0.,-1.)) ;
#2614 = DIRECTION('center_axis',(0.,1.,0.)) ;
#2615 = DIRECTION('ref_axis',(0.,0.,1.)) ;
#2616 = DIRECTION('',(0.,0.,-1.)) ;
#2617 = DIRECTION('center_axis',(-1.,0.,0.)) ;
#2618 = DIRECTION('ref_axis',(0.,0.,1.)) ;
#2619 = DIRECTION('',(0.,0.,-1.)) ;
#2620 = DIRECTION('center_axis',(-7.43452918275775E-17,-1.,0.)) ;
#2621 = DIRECTION('ref_axis',(1.,-7.43452918275775E-17,0.)) ;
#2622 = DIRECTION('axis',(0.,0.,1.)) ;
#2623 = DIRECTION('refdir',(1.,0.,0.)) ;
#2624 = DIRECTION('center_axis',(1.58603289232165E-16,-1.,0.)) ;
#2625 = DIRECTION('ref_axis',(1.,1.58603289232165E-16,0.)) ;
#2626 = DIRECTION('',(-1.,-1.58603289232165E-16,0.)) ;
#2627 = DIRECTION('',(0.,0.,-1.)) ;
#2628 = DIRECTION('',(-1.,-1.58603289232165E-16,0.)) ;
#2629 = DIRECTION('',(0.,0.,-1.)) ;
#2630 = DIRECTION('center_axis',(-1.,0.,0.)) ;
#2631 = DIRECTION('ref_axis',(0.,0.,1.)) ;
#2632 = DIRECTION('',(0.,1.,0.)) ;
#2633 = DIRECTION('',(0.,0.,-1.)) ;
#2634 = DIRECTION('',(0.,1.,0.)) ;
#2635 = DIRECTION('center_axis',(1.05735526154777E-16,-1.,0.)) ;
#2636 = DIRECTION('ref_axis',(1.,1.05735526154777E-16,0.)) ;
#2637 = DIRECTION('',(-1.,-1.05735526154777E-16,0.)) ;
#2638 = DIRECTION('',(0.,0.,-1.)) ;
#2639 = DIRECTION('',(-1.,-1.05735526154777E-16,0.)) ;
#2640 = DIRECTION('center_axis',(-1.,0.,0.)) ;
#2641 = DIRECTION('ref_axis',(0.,0.,1.)) ;
#2642 = DIRECTION('',(0.,1.,0.)) ;
#2643 = DIRECTION('',(0.,1.,0.)) ;
#2644 = DIRECTION('center_axis',(0.,0.,-1.)) ;
#2645 = DIRECTION('ref_axis',(-1.,0.,0.)) ;
#2646 = DIRECTION('',(1.,-1.23908819712629E-16,0.)) ;
#2647 = DIRECTION('',(0.,-1.,0.)) ;
#2648 = DIRECTION('',(-1.,1.23908819712629E-16,0.)) ;
#2649 = DIRECTION('',(0.,1.,0.)) ;
#2650 = DIRECTION('',(-1.,0.,0.)) ;
#2651 = DIRECTION('',(0.,1.,0.)) ;
#2652 = DIRECTION('',(1.,0.,0.)) ;
#2653 = DIRECTION('',(0.,-1.,0.)) ;
#2654 = DIRECTION('center_axis',(-1.,0.,0.)) ;
#2655 = DIRECTION('ref_axis',(0.,0.,1.)) ;
#2656 = DIRECTION('',(0.,1.,0.)) ;
#2657 = DIRECTION('',(0.,0.,-1.)) ;
#2658 = DIRECTION('',(0.,1.,0.)) ;
#2659 = DIRECTION('',(0.,0.,1.)) ;
#2660 = DIRECTION('center_axis',(1.26391510089385E-16,-1.,0.)) ;
#2661 = DIRECTION('ref_axis',(1.,1.26391510089385E-16,0.)) ;
#2662 = DIRECTION('',(-1.,-1.26391510089385E-16,0.)) ;
#2663 = DIRECTION('',(0.,0.,1.)) ;
#2664 = DIRECTION('',(-1.,-1.26391510089385E-16,0.)) ;
#2665 = DIRECTION('',(0.,0.,-1.)) ;
#2666 = DIRECTION('center_axis',(-1.,0.,0.)) ;
#2667 = DIRECTION('ref_axis',(0.,0.,1.)) ;
#2668 = DIRECTION('',(0.,1.,0.)) ;
#2669 = DIRECTION('',(0.,0.,1.)) ;
#2670 = DIRECTION('',(0.,1.,0.)) ;
#2671 = DIRECTION('',(0.,0.,-1.)) ;
#2672 = DIRECTION('center_axis',(1.51669812107262E-16,-1.,0.)) ;
#2673 = DIRECTION('ref_axis',(1.,1.51669812107262E-16,0.)) ;
#2674 = DIRECTION('',(-1.,-1.51669812107262E-16,0.)) ;
#2675 = DIRECTION('',(0.,0.,1.)) ;
#2676 = DIRECTION('',(-1.,-1.51669812107262E-16,0.)) ;
#2677 = DIRECTION('',(0.,0.,-1.)) ;
#2678 = DIRECTION('center_axis',(0.,0.,1.)) ;
#2679 = DIRECTION('ref_axis',(1.,0.,0.)) ;
#2680 = DIRECTION('center_axis',(0.,0.,1.)) ;
#2681 = DIRECTION('ref_axis',(1.,0.,0.)) ;
#2682 = DIRECTION('center_axis',(0.,0.,1.)) ;
#2683 = DIRECTION('ref_axis',(1.,0.,0.)) ;
#2684 = DIRECTION('center_axis',(0.,0.,1.)) ;
#2685 = DIRECTION('ref_axis',(1.,0.,0.)) ;
#2686 = DIRECTION('center_axis',(0.,0.,1.)) ;
#2687 = DIRECTION('ref_axis',(1.,0.,0.)) ;
#2688 = DIRECTION('center_axis',(0.,0.,-1.)) ;
#2689 = DIRECTION('ref_axis',(-1.,0.,0.)) ;
#2690 = DIRECTION('center_axis',(0.,0.,-1.)) ;
#2691 = DIRECTION('ref_axis',(-1.,0.,0.)) ;
#2692 = DIRECTION('center_axis',(0.,0.,-1.)) ;
#2693 = DIRECTION('ref_axis',(-1.,0.,0.)) ;
#2694 = DIRECTION('center_axis',(0.,0.,-1.)) ;
#2695 = DIRECTION('ref_axis',(-1.,0.,0.)) ;
#2696 = DIRECTION('center_axis',(0.,0.,-1.)) ;
#2697 = DIRECTION('ref_axis',(-1.,0.,0.)) ;
#2698 = DIRECTION('',(0.,-1.,0.)) ;
#2699 = DIRECTION('',(1.,-1.23908819712629E-16,0.)) ;
#2700 = DIRECTION('',(0.,1.,0.)) ;
#2701 = DIRECTION('',(-1.,1.23908819712629E-16,0.)) ;
#2702 = DIRECTION('',(0.,1.,0.)) ;
#2703 = DIRECTION('',(-1.,0.,0.)) ;
#2704 = DIRECTION('',(0.,-1.,0.)) ;
#2705 = DIRECTION('',(1.,0.,0.)) ;
#2706 = DIRECTION('center_axis',(0.,0.,1.)) ;
#2707 = DIRECTION('ref_axis',(1.,0.,0.)) ;
#2708 = DIRECTION('center_axis',(0.,0.,-1.)) ;
#2709 = DIRECTION('ref_axis',(-1.,0.,0.)) ;
#2710 = DIRECTION('center_axis',(0.,0.,1.)) ;
#2711 = DIRECTION('ref_axis',(1.,0.,0.)) ;
#2712 = DIRECTION('center_axis',(0.,0.,-1.)) ;
#2713 = DIRECTION('ref_axis',(-1.,0.,0.)) ;
#2714 = DIRECTION('center_axis',(-1.,0.,0.)) ;
#2715 = DIRECTION('ref_axis',(0.,0.,1.)) ;
#2716 = DIRECTION('',(0.,0.,-1.)) ;
#2717 = DIRECTION('',(0.,0.,-1.)) ;
#2718 = DIRECTION('center_axis',(0.,-1.,0.)) ;
#2719 = DIRECTION('ref_axis',(0.,0.,-1.)) ;
#2720 = DIRECTION('',(0.,0.,-1.)) ;
#2721 = DIRECTION('center_axis',(1.,0.,0.)) ;
#2722 = DIRECTION('ref_axis',(0.,0.,-1.)) ;
#2723 = DIRECTION('',(0.,0.,-1.)) ;
#2724 = DIRECTION('center_axis',(0.,1.,0.)) ;
#2725 = DIRECTION('ref_axis',(0.,0.,1.)) ;
#2726 = DIRECTION('center_axis',(1.,0.,0.)) ;
#2727 = DIRECTION('ref_axis',(0.,0.,-1.)) ;
#2728 = DIRECTION('',(0.,0.,-1.)) ;
#2729 = DIRECTION('',(0.,0.,-1.)) ;
#2730 = DIRECTION('center_axis',(1.23908819712629E-16,1.,0.)) ;
#2731 = DIRECTION('ref_axis',(-1.,1.23908819712629E-16,0.)) ;
#2732 = DIRECTION('',(0.,0.,-1.)) ;
#2733 = DIRECTION('center_axis',(-1.,0.,0.)) ;
#2734 = DIRECTION('ref_axis',(0.,0.,1.)) ;
#2735 = DIRECTION('',(0.,0.,-1.)) ;
#2736 = DIRECTION('center_axis',(-1.23908819712629E-16,-1.,0.)) ;
#2737 = DIRECTION('ref_axis',(1.,-1.23908819712629E-16,0.)) ;
#2738 = DIRECTION('axis',(0.,0.,1.)) ;
#2739 = DIRECTION('refdir',(1.,0.,0.)) ;
#2740 = DIRECTION('center_axis',(1.58603289232165E-16,-1.,0.)) ;
#2741 = DIRECTION('ref_axis',(1.,1.58603289232165E-16,0.)) ;
#2742 = DIRECTION('',(-1.,-1.58603289232165E-16,0.)) ;
#2743 = DIRECTION('',(0.,0.,-1.)) ;
#2744 = DIRECTION('',(-1.,-1.58603289232165E-16,0.)) ;
#2745 = DIRECTION('',(0.,0.,-1.)) ;
#2746 = DIRECTION('center_axis',(-1.,0.,0.)) ;
#2747 = DIRECTION('ref_axis',(0.,0.,1.)) ;
#2748 = DIRECTION('',(0.,1.,0.)) ;
#2749 = DIRECTION('',(0.,0.,-1.)) ;
#2750 = DIRECTION('',(0.,1.,0.)) ;
#2751 = DIRECTION('center_axis',(1.05735526154777E-16,-1.,0.)) ;
#2752 = DIRECTION('ref_axis',(1.,1.05735526154777E-16,0.)) ;
#2753 = DIRECTION('',(-1.,-1.05735526154777E-16,0.)) ;
#2754 = DIRECTION('',(0.,0.,-1.)) ;
#2755 = DIRECTION('',(-1.,-1.05735526154777E-16,0.)) ;
#2756 = DIRECTION('center_axis',(-1.,0.,0.)) ;
#2757 = DIRECTION('ref_axis',(0.,0.,1.)) ;
#2758 = DIRECTION('',(0.,1.,0.)) ;
#2759 = DIRECTION('',(0.,1.,0.)) ;
#2760 = DIRECTION('center_axis',(0.,0.,-1.)) ;
#2761 = DIRECTION('ref_axis',(-1.,0.,0.)) ;
#2762 = DIRECTION('',(1.,-9.91270557701033E-17,0.)) ;
#2763 = DIRECTION('',(0.,-1.,0.)) ;
#2764 = DIRECTION('',(-1.,1.48690583655155E-16,0.)) ;
#2765 = DIRECTION('',(0.,1.,0.)) ;
#2766 = DIRECTION('center_axis',(-1.,0.,0.)) ;
#2767 = DIRECTION('ref_axis',(0.,0.,1.)) ;
#2768 = DIRECTION('',(0.,1.,0.)) ;
#2769 = DIRECTION('',(0.,0.,-1.)) ;
#2770 = DIRECTION('',(0.,1.,0.)) ;
#2771 = DIRECTION('',(0.,0.,1.)) ;
#2772 = DIRECTION('center_axis',(1.26391510089385E-16,-1.,0.)) ;
#2773 = DIRECTION('ref_axis',(1.,1.26391510089385E-16,0.)) ;
#2774 = DIRECTION('',(-1.,-1.26391510089385E-16,0.)) ;
#2775 = DIRECTION('',(0.,0.,1.)) ;
#2776 = DIRECTION('',(-1.,-1.26391510089385E-16,0.)) ;
#2777 = DIRECTION('',(0.,0.,-1.)) ;
#2778 = DIRECTION('center_axis',(-1.,0.,0.)) ;
#2779 = DIRECTION('ref_axis',(0.,0.,1.)) ;
#2780 = DIRECTION('',(0.,1.,0.)) ;
#2781 = DIRECTION('',(0.,0.,1.)) ;
#2782 = DIRECTION('',(0.,1.,0.)) ;
#2783 = DIRECTION('',(0.,0.,-1.)) ;
#2784 = DIRECTION('center_axis',(1.51669812107262E-16,-1.,0.)) ;
#2785 = DIRECTION('ref_axis',(1.,1.51669812107262E-16,0.)) ;
#2786 = DIRECTION('',(-1.,-1.51669812107262E-16,0.)) ;
#2787 = DIRECTION('',(0.,0.,1.)) ;
#2788 = DIRECTION('',(-1.,-1.51669812107262E-16,0.)) ;
#2789 = DIRECTION('',(0.,0.,-1.)) ;
#2790 = DIRECTION('center_axis',(0.,0.,1.)) ;
#2791 = DIRECTION('ref_axis',(1.,0.,0.)) ;
#2792 = DIRECTION('center_axis',(0.,0.,1.)) ;
#2793 = DIRECTION('ref_axis',(1.,0.,0.)) ;
#2794 = DIRECTION('center_axis',(0.,0.,1.)) ;
#2795 = DIRECTION('ref_axis',(1.,0.,0.)) ;
#2796 = DIRECTION('center_axis',(0.,0.,1.)) ;
#2797 = DIRECTION('ref_axis',(1.,0.,0.)) ;
#2798 = DIRECTION('center_axis',(0.,0.,1.)) ;
#2799 = DIRECTION('ref_axis',(1.,0.,0.)) ;
#2800 = DIRECTION('center_axis',(0.,0.,-1.)) ;
#2801 = DIRECTION('ref_axis',(-1.,0.,0.)) ;
#2802 = DIRECTION('center_axis',(0.,0.,-1.)) ;
#2803 = DIRECTION('ref_axis',(-1.,0.,0.)) ;
#2804 = DIRECTION('center_axis',(0.,0.,-1.)) ;
#2805 = DIRECTION('ref_axis',(-1.,0.,0.)) ;
#2806 = DIRECTION('center_axis',(0.,0.,-1.)) ;
#2807 = DIRECTION('ref_axis',(-1.,0.,0.)) ;
#2808 = DIRECTION('center_axis',(0.,0.,-1.)) ;
#2809 = DIRECTION('ref_axis',(-1.,0.,0.)) ;
#2810 = DIRECTION('',(0.,-1.,0.)) ;
#2811 = DIRECTION('',(1.,-9.91270557701033E-17,0.)) ;
#2812 = DIRECTION('',(0.,1.,0.)) ;
#2813 = DIRECTION('',(-1.,1.48690583655155E-16,0.)) ;
#2814 = DIRECTION('center_axis',(0.,0.,1.)) ;
#2815 = DIRECTION('ref_axis',(1.,0.,0.)) ;
#2816 = DIRECTION('center_axis',(0.,0.,-1.)) ;
#2817 = DIRECTION('ref_axis',(-1.,0.,0.)) ;
#2818 = DIRECTION('center_axis',(0.,0.,1.)) ;
#2819 = DIRECTION('ref_axis',(1.,0.,0.)) ;
#2820 = DIRECTION('center_axis',(0.,0.,-1.)) ;
#2821 = DIRECTION('ref_axis',(-1.,0.,0.)) ;
#2822 = DIRECTION('center_axis',(1.,0.,0.)) ;
#2823 = DIRECTION('ref_axis',(0.,0.,-1.)) ;
#2824 = DIRECTION('',(0.,0.,-1.)) ;
#2825 = DIRECTION('',(0.,0.,-1.)) ;
#2826 = DIRECTION('center_axis',(9.91270557701033E-17,1.,0.)) ;
#2827 = DIRECTION('ref_axis',(-1.,9.91270557701033E-17,0.)) ;
#2828 = DIRECTION('',(0.,0.,-1.)) ;
#2829 = DIRECTION('center_axis',(-1.,0.,0.)) ;
#2830 = DIRECTION('ref_axis',(0.,0.,1.)) ;
#2831 = DIRECTION('',(0.,0.,-1.)) ;
#2832 = DIRECTION('center_axis',(-1.48690583655155E-16,-1.,0.)) ;
#2833 = DIRECTION('ref_axis',(1.,-1.48690583655155E-16,0.)) ;
#2834 = DIRECTION('axis',(0.,0.,1.)) ;
#2835 = DIRECTION('refdir',(1.,0.,0.)) ;
#2836 = DIRECTION('center_axis',(1.05735526154777E-16,-1.,0.)) ;
#2837 = DIRECTION('ref_axis',(1.,1.05735526154777E-16,0.)) ;
#2838 = DIRECTION('',(-1.,-1.05735526154777E-16,0.)) ;
#2839 = DIRECTION('',(0.,0.,-1.)) ;
#2840 = DIRECTION('',(-1.,-1.05735526154777E-16,0.)) ;
#2841 = DIRECTION('',(0.,0.,-1.)) ;
#2842 = DIRECTION('center_axis',(-1.,0.,0.)) ;
#2843 = DIRECTION('ref_axis',(0.,0.,1.)) ;
#2844 = DIRECTION('',(0.,1.,0.)) ;
#2845 = DIRECTION('',(0.,0.,-1.)) ;
#2846 = DIRECTION('',(0.,1.,0.)) ;
#2847 = DIRECTION('center_axis',(1.05735526154777E-16,-1.,0.)) ;
#2848 = DIRECTION('ref_axis',(1.,1.05735526154777E-16,0.)) ;
#2849 = DIRECTION('',(-1.,-1.05735526154777E-16,0.)) ;
#2850 = DIRECTION('',(0.,0.,-1.)) ;
#2851 = DIRECTION('',(-1.,-1.05735526154777E-16,0.)) ;
#2852 = DIRECTION('center_axis',(-1.,0.,0.)) ;
#2853 = DIRECTION('ref_axis',(0.,0.,1.)) ;
#2854 = DIRECTION('',(0.,1.,0.)) ;
#2855 = DIRECTION('',(0.,1.,0.)) ;
#2856 = DIRECTION('center_axis',(0.,0.,-1.)) ;
#2857 = DIRECTION('ref_axis',(-1.,0.,0.)) ;
#2858 = DIRECTION('center_axis',(-1.,0.,0.)) ;
#2859 = DIRECTION('ref_axis',(0.,0.,1.)) ;
#2860 = DIRECTION('',(0.,1.,0.)) ;
#2861 = DIRECTION('',(0.,0.,-1.)) ;
#2862 = DIRECTION('',(0.,1.,0.)) ;
#2863 = DIRECTION('',(0.,0.,1.)) ;
#2864 = DIRECTION('center_axis',(1.01113208071508E-16,-1.,0.)) ;
#2865 = DIRECTION('ref_axis',(1.,1.01113208071508E-16,0.)) ;
#2866 = DIRECTION('',(-1.,-1.01113208071508E-16,0.)) ;
#2867 = DIRECTION('',(0.,0.,1.)) ;
#2868 = DIRECTION('',(-1.,-1.01113208071508E-16,0.)) ;
#2869 = DIRECTION('',(0.,0.,-1.)) ;
#2870 = DIRECTION('center_axis',(-1.,0.,0.)) ;
#2871 = DIRECTION('ref_axis',(0.,0.,1.)) ;
#2872 = DIRECTION('',(0.,1.,0.)) ;
#2873 = DIRECTION('',(0.,0.,1.)) ;
#2874 = DIRECTION('',(0.,1.,0.)) ;
#2875 = DIRECTION('',(0.,0.,-1.)) ;
#2876 = DIRECTION('center_axis',(1.51669812107262E-16,-1.,0.)) ;
#2877 = DIRECTION('ref_axis',(1.,1.51669812107262E-16,0.)) ;
#2878 = DIRECTION('',(-1.,-1.51669812107262E-16,0.)) ;
#2879 = DIRECTION('',(0.,0.,1.)) ;
#2880 = DIRECTION('',(-1.,-1.51669812107262E-16,0.)) ;
#2881 = DIRECTION('',(0.,0.,-1.)) ;
#2882 = DIRECTION('center_axis',(0.,0.,1.)) ;
#2883 = DIRECTION('ref_axis',(1.,0.,0.)) ;
#2884 = DIRECTION('center_axis',(0.,0.,1.)) ;
#2885 = DIRECTION('ref_axis',(1.,0.,0.)) ;
#2886 = DIRECTION('center_axis',(0.,0.,1.)) ;
#2887 = DIRECTION('ref_axis',(1.,0.,0.)) ;
#2888 = DIRECTION('center_axis',(0.,0.,1.)) ;
#2889 = DIRECTION('ref_axis',(1.,0.,0.)) ;
#2890 = DIRECTION('center_axis',(0.,0.,1.)) ;
#2891 = DIRECTION('ref_axis',(1.,0.,0.)) ;
#2892 = DIRECTION('center_axis',(0.,0.,-1.)) ;
#2893 = DIRECTION('ref_axis',(-1.,0.,0.)) ;
#2894 = DIRECTION('center_axis',(0.,0.,-1.)) ;
#2895 = DIRECTION('ref_axis',(-1.,0.,0.)) ;
#2896 = DIRECTION('center_axis',(0.,0.,-1.)) ;
#2897 = DIRECTION('ref_axis',(-1.,0.,0.)) ;
#2898 = DIRECTION('center_axis',(0.,0.,-1.)) ;
#2899 = DIRECTION('ref_axis',(-1.,0.,0.)) ;
#2900 = DIRECTION('center_axis',(0.,0.,-1.)) ;
#2901 = DIRECTION('ref_axis',(-1.,0.,0.)) ;
#2902 = DIRECTION('center_axis',(0.,0.,1.)) ;
#2903 = DIRECTION('ref_axis',(1.,0.,0.)) ;
#2904 = DIRECTION('center_axis',(0.,0.,-1.)) ;
#2905 = DIRECTION('ref_axis',(-1.,0.,0.)) ;
#2906 = DIRECTION('center_axis',(0.,0.,1.)) ;
#2907 = DIRECTION('ref_axis',(1.,0.,0.)) ;
#2908 = DIRECTION('center_axis',(0.,0.,-1.)) ;
#2909 = DIRECTION('ref_axis',(-1.,0.,0.)) ;
#2910 = DIRECTION('axis',(0.,0.,1.)) ;
#2911 = DIRECTION('refdir',(1.,0.,0.)) ;
#2912 = DIRECTION('center_axis',(-1.,-3.70074341541719E-16,0.)) ;
#2913 = DIRECTION('ref_axis',(3.70074341541719E-16,-1.,0.)) ;
#2914 = DIRECTION('',(-3.70074341541719E-16,1.,0.)) ;
#2915 = DIRECTION('',(0.,0.,-1.)) ;
#2916 = DIRECTION('',(3.70074341541719E-16,-1.,0.)) ;
#2917 = DIRECTION('',(0.,0.,-1.)) ;
#2918 = DIRECTION('center_axis',(0.,-1.,0.)) ;
#2919 = DIRECTION('ref_axis',(0.,0.,-1.)) ;
#2920 = DIRECTION('',(-1.,0.,0.)) ;
#2921 = DIRECTION('',(1.,0.,0.)) ;
#2922 = DIRECTION('',(0.,0.,-1.)) ;
#2923 = DIRECTION('center_axis',(1.,3.70074341541719E-16,0.)) ;
#2924 = DIRECTION('ref_axis',(-3.70074341541719E-16,1.,0.)) ;
#2925 = DIRECTION('',(3.70074341541719E-16,-1.,0.)) ;
#2926 = DIRECTION('',(-3.70074341541719E-16,1.,0.)) ;
#2927 = DIRECTION('',(0.,0.,-1.)) ;
#2928 = DIRECTION('center_axis',(0.,1.,0.)) ;
#2929 = DIRECTION('ref_axis',(0.,0.,1.)) ;
#2930 = DIRECTION('',(1.,0.,0.)) ;
#2931 = DIRECTION('',(-1.,0.,0.)) ;
#2932 = DIRECTION('center_axis',(0.,0.,1.)) ;
#2933 = DIRECTION('ref_axis',(1.,0.,0.)) ;
#2934 = DIRECTION('',(-3.70074341541719E-16,1.,0.)) ;
#2935 = DIRECTION('',(-1.,0.,0.)) ;
#2936 = DIRECTION('',(3.70074341541719E-16,-1.,0.)) ;
#2937 = DIRECTION('',(1.,0.,0.)) ;
#2938 = DIRECTION('center_axis',(0.,0.,1.)) ;
#2939 = DIRECTION('ref_axis',(1.,0.,0.)) ;
#2940 = DIRECTION('',(-3.70074341541719E-16,1.,0.)) ;
#2941 = DIRECTION('',(1.,0.,0.)) ;
#2942 = DIRECTION('',(3.70074341541719E-16,-1.,0.)) ;
#2943 = DIRECTION('',(-1.,0.,0.)) ;
#2944 = DIRECTION('',(-3.70074341541719E-16,1.,0.)) ;
#2945 = DIRECTION('',(-1.,0.,0.)) ;
#2946 = DIRECTION('',(3.70074341541719E-16,-1.,0.)) ;
#2947 = DIRECTION('',(1.,0.,0.)) ;
#2948 = DIRECTION('center_axis',(-1.,-3.70074341541719E-16,0.)) ;
#2949 = DIRECTION('ref_axis',(3.70074341541719E-16,-1.,0.)) ;
#2950 = DIRECTION('',(0.,0.,-1.)) ;
#2951 = DIRECTION('',(0.,0.,-1.)) ;
#2952 = DIRECTION('center_axis',(0.,-1.,0.)) ;
#2953 = DIRECTION('ref_axis',(0.,0.,-1.)) ;
#2954 = DIRECTION('',(0.,0.,-1.)) ;
#2955 = DIRECTION('center_axis',(1.,3.70074341541719E-16,0.)) ;
#2956 = DIRECTION('ref_axis',(-3.70074341541719E-16,1.,0.)) ;
#2957 = DIRECTION('',(0.,0.,-1.)) ;
#2958 = DIRECTION('center_axis',(0.,1.,0.)) ;
#2959 = DIRECTION('ref_axis',(0.,0.,1.)) ;
#2960 = DIRECTION('center_axis',(-1.,-3.70074341541719E-16,0.)) ;
#2961 = DIRECTION('ref_axis',(3.70074341541719E-16,-1.,0.)) ;
#2962 = DIRECTION('',(0.,0.,-1.)) ;
#2963 = DIRECTION('',(0.,0.,-1.)) ;
#2964 = DIRECTION('',(-3.70074341541719E-16,1.,0.)) ;
#2965 = DIRECTION('center_axis',(0.,-1.,0.)) ;
#2966 = DIRECTION('ref_axis',(0.,0.,-1.)) ;
#2967 = DIRECTION('',(0.,0.,-1.)) ;
#2968 = DIRECTION('',(-1.,0.,0.)) ;
#2969 = DIRECTION('center_axis',(1.,3.70074341541719E-16,0.)) ;
#2970 = DIRECTION('ref_axis',(-3.70074341541719E-16,1.,0.)) ;
#2971 = DIRECTION('',(0.,0.,-1.)) ;
#2972 = DIRECTION('',(3.70074341541719E-16,-1.,0.)) ;
#2973 = DIRECTION('center_axis',(0.,1.,0.)) ;
#2974 = DIRECTION('ref_axis',(0.,0.,1.)) ;
#2975 = DIRECTION('',(1.,0.,0.)) ;
#2976 = DIRECTION('center_axis',(0.,0.,1.)) ;
#2977 = DIRECTION('ref_axis',(1.,0.,0.)) ;
#2978 = DIRECTION('',(3.70074341541719E-16,-1.,0.)) ;
#2979 = DIRECTION('',(1.,0.,0.)) ;
#2980 = DIRECTION('',(-3.70074341541719E-16,1.,0.)) ;
#2981 = DIRECTION('',(-1.,0.,0.)) ;
#2982 = DIRECTION('center_axis',(0.,0.,1.)) ;
#2983 = DIRECTION('ref_axis',(1.,0.,0.)) ;
#2984 = DIRECTION('',(3.70074341541719E-16,-1.,0.)) ;
#2985 = DIRECTION('',(-1.,0.,0.)) ;
#2986 = DIRECTION('',(-3.70074341541719E-16,1.,0.)) ;
#2987 = DIRECTION('',(1.,0.,0.)) ;
#2988 = DIRECTION('center_axis',(-1.,-3.70074341541719E-16,0.)) ;
#2989 = DIRECTION('ref_axis',(3.70074341541719E-16,-1.,0.)) ;
#2990 = DIRECTION('',(0.,0.,1.)) ;
#2991 = DIRECTION('',(0.,0.,1.)) ;
#2992 = DIRECTION('center_axis',(0.,1.,0.)) ;
#2993 = DIRECTION('ref_axis',(0.,0.,1.)) ;
#2994 = DIRECTION('',(0.,0.,1.)) ;
#2995 = DIRECTION('center_axis',(1.,3.70074341541719E-16,0.)) ;
#2996 = DIRECTION('ref_axis',(-3.70074341541719E-16,1.,0.)) ;
#2997 = DIRECTION('',(0.,0.,1.)) ;
#2998 = DIRECTION('center_axis',(0.,-1.,0.)) ;
#2999 = DIRECTION('ref_axis',(0.,0.,-1.)) ;
#3000 = DIRECTION('axis',(0.,0.,1.)) ;
#3001 = DIRECTION('refdir',(1.,0.,0.)) ;
#3002 = DIRECTION('center_axis',(-1.,4.62592926927149E-16,0.)) ;
#3003 = DIRECTION('ref_axis',(-4.62592926927149E-16,-1.,0.)) ;
#3004 = DIRECTION('',(4.62592926927149E-16,1.,0.)) ;
#3005 = DIRECTION('',(0.,0.,-1.)) ;
#3006 = DIRECTION('',(-4.62592926927149E-16,-1.,0.)) ;
#3007 = DIRECTION('',(0.,0.,-1.)) ;
#3008 = DIRECTION('center_axis',(0.,-1.,0.)) ;
#3009 = DIRECTION('ref_axis',(0.,0.,-1.)) ;
#3010 = DIRECTION('',(-1.,0.,0.)) ;
#3011 = DIRECTION('',(1.,0.,0.)) ;
#3012 = DIRECTION('',(0.,0.,-1.)) ;
#3013 = DIRECTION('center_axis',(1.,-4.62592926927149E-16,0.)) ;
#3014 = DIRECTION('ref_axis',(4.62592926927149E-16,1.,0.)) ;
#3015 = DIRECTION('',(-4.62592926927149E-16,-1.,0.)) ;
#3016 = DIRECTION('',(4.62592926927149E-16,1.,0.)) ;
#3017 = DIRECTION('',(0.,0.,-1.)) ;
#3018 = DIRECTION('center_axis',(0.,1.,0.)) ;
#3019 = DIRECTION('ref_axis',(0.,0.,1.)) ;
#3020 = DIRECTION('',(1.,0.,0.)) ;
#3021 = DIRECTION('',(-1.,0.,0.)) ;
#3022 = DIRECTION('center_axis',(0.,0.,1.)) ;
#3023 = DIRECTION('ref_axis',(1.,0.,0.)) ;
#3024 = DIRECTION('',(4.62592926927149E-16,1.,0.)) ;
#3025 = DIRECTION('',(-1.,0.,0.)) ;
#3026 = DIRECTION('',(-4.62592926927149E-16,-1.,0.)) ;
#3027 = DIRECTION('',(1.,0.,0.)) ;
#3028 = DIRECTION('center_axis',(0.,0.,1.)) ;
#3029 = DIRECTION('ref_axis',(1.,0.,0.)) ;
#3030 = DIRECTION('',(4.62592926927149E-16,1.,0.)) ;
#3031 = DIRECTION('',(1.,0.,0.)) ;
#3032 = DIRECTION('',(-4.62592926927149E-16,-1.,0.)) ;
#3033 = DIRECTION('',(-1.,0.,0.)) ;
#3034 = DIRECTION('',(4.62592926927149E-16,1.,0.)) ;
#3035 = DIRECTION('',(-1.,0.,0.)) ;
#3036 = DIRECTION('',(-4.62592926927149E-16,-1.,0.)) ;
#3037 = DIRECTION('',(1.,0.,0.)) ;
#3038 = DIRECTION('center_axis',(-1.,4.62592926927149E-16,0.)) ;
#3039 = DIRECTION('ref_axis',(-4.62592926927149E-16,-1.,0.)) ;
#3040 = DIRECTION('',(0.,0.,-1.)) ;
#3041 = DIRECTION('',(0.,0.,-1.)) ;
#3042 = DIRECTION('center_axis',(0.,-1.,0.)) ;
#3043 = DIRECTION('ref_axis',(0.,0.,-1.)) ;
#3044 = DIRECTION('',(0.,0.,-1.)) ;
#3045 = DIRECTION('center_axis',(1.,-4.62592926927149E-16,0.)) ;
#3046 = DIRECTION('ref_axis',(4.62592926927149E-16,1.,0.)) ;
#3047 = DIRECTION('',(0.,0.,-1.)) ;
#3048 = DIRECTION('center_axis',(0.,1.,0.)) ;
#3049 = DIRECTION('ref_axis',(0.,0.,1.)) ;
#3050 = DIRECTION('center_axis',(-1.,4.62592926927149E-16,0.)) ;
#3051 = DIRECTION('ref_axis',(-4.62592926927149E-16,-1.,0.)) ;
#3052 = DIRECTION('',(0.,0.,-1.)) ;
#3053 = DIRECTION('',(0.,0.,-1.)) ;
#3054 = DIRECTION('',(4.62592926927149E-16,1.,0.)) ;
#3055 = DIRECTION('center_axis',(0.,-1.,0.)) ;
#3056 = DIRECTION('ref_axis',(0.,0.,-1.)) ;
#3057 = DIRECTION('',(0.,0.,-1.)) ;
#3058 = DIRECTION('',(-1.,0.,0.)) ;
#3059 = DIRECTION('center_axis',(1.,-4.62592926927149E-16,0.)) ;
#3060 = DIRECTION('ref_axis',(4.62592926927149E-16,1.,0.)) ;
#3061 = DIRECTION('',(0.,0.,-1.)) ;
#3062 = DIRECTION('',(-4.62592926927149E-16,-1.,0.)) ;
#3063 = DIRECTION('center_axis',(0.,1.,0.)) ;
#3064 = DIRECTION('ref_axis',(0.,0.,1.)) ;
#3065 = DIRECTION('',(1.,0.,0.)) ;
#3066 = DIRECTION('center_axis',(0.,0.,1.)) ;
#3067 = DIRECTION('ref_axis',(1.,0.,0.)) ;
#3068 = DIRECTION('',(-4.62592926927149E-16,-1.,0.)) ;
#3069 = DIRECTION('',(1.,0.,0.)) ;
#3070 = DIRECTION('',(4.62592926927149E-16,1.,0.)) ;
#3071 = DIRECTION('',(-1.,0.,0.)) ;
#3072 = DIRECTION('center_axis',(0.,0.,1.)) ;
#3073 = DIRECTION('ref_axis',(1.,0.,0.)) ;
#3074 = DIRECTION('',(-4.62592926927149E-16,-1.,0.)) ;
#3075 = DIRECTION('',(-1.,0.,0.)) ;
#3076 = DIRECTION('',(4.62592926927149E-16,1.,0.)) ;
#3077 = DIRECTION('',(1.,0.,0.)) ;
#3078 = DIRECTION('center_axis',(-1.,4.62592926927149E-16,0.)) ;
#3079 = DIRECTION('ref_axis',(-4.62592926927149E-16,-1.,0.)) ;
#3080 = DIRECTION('',(0.,0.,1.)) ;
#3081 = DIRECTION('',(0.,0.,1.)) ;
#3082 = DIRECTION('center_axis',(0.,1.,0.)) ;
#3083 = DIRECTION('ref_axis',(0.,0.,1.)) ;
#3084 = DIRECTION('',(0.,0.,1.)) ;
#3085 = DIRECTION('center_axis',(1.,-4.62592926927149E-16,0.)) ;
#3086 = DIRECTION('ref_axis',(4.62592926927149E-16,1.,0.)) ;
#3087 = DIRECTION('',(0.,0.,1.)) ;
#3088 = DIRECTION('center_axis',(0.,-1.,0.)) ;
#3089 = DIRECTION('ref_axis',(0.,0.,-1.)) ;
#3090 = DIRECTION('',(6.88338275267608E-15,-6.7753148020865E-18,-1.)) ;
#3091 = DIRECTION('',(-1.,5.55111512311821E-17,-6.88338275267608E-15)) ;
#3092 = DIRECTION('',(1.,-5.55111512311821E-17,1.21291865440292E-14)) ;
#3093 = DIRECTION('',(1.21291865440292E-14,-8.32667268469016E-17,-1.)) ;
#3094 = DIRECTION('',(-1.,5.55111512311821E-17,-6.77236045021284E-15)) ;
#3095 = DIRECTION('',(-6.77236045021284E-15,-8.32667268468803E-17,1.)) ;
#3096 = DIRECTION('',(-1.83186799063143E-15,-1.,-2.05488152929729E-17)) ;
#3097 = DIRECTION('',(1.38777878077486E-16,-2.05488152929732E-17,1.)) ;
#3098 = DIRECTION('',(-1.,5.55111512311821E-17,-1.2073675392798E-14)) ;
#3099 = DIRECTION('',(-1.2073675392798E-14,6.29798808536556E-17,1.)) ;
#3100 = DIRECTION('',(6.88338275267607E-15,4.163336342343E-17,-1.)) ;
#3101 = DIRECTION('',(-1.,4.99600361081264E-16,-6.88338275267607E-15)) ;
#3102 = DIRECTION('',(-1.,5.55111512311821E-17,-1.2073675392798E-14)) ;
#3103 = DIRECTION('',(-1.2073675392798E-14,3.85463322789439E-29,1.)) ;
#3104 = DIRECTION('',(-1.,5.55111512311821E-17,-1.2073675392798E-14)) ;
#3105 = DIRECTION('',(-1.2073675392798E-14,6.29798808536556E-17,1.)) ;
#3106 = DIRECTION('',(6.88338275267607E-15,4.163336342343E-17,-1.)) ;
#3107 = DIRECTION('',(-1.,4.99600361081264E-16,-6.88338275267607E-15)) ;
#3108 = CARTESIAN_POINT('',(0.,0.,0.)) ;
#3109 = CARTESIAN_POINT('',(0.,0.,0.)) ;
#3110 = CARTESIAN_POINT('Origin',(32.5,-19.4,5.)) ;
#3111 = CARTESIAN_POINT('',(32.5,-19.4,1.9)) ;
#3112 = CARTESIAN_POINT('',(-32.5,-19.4,1.9)) ;
#3113 = CARTESIAN_POINT('',(32.5,-19.4,1.9)) ;
#3114 = CARTESIAN_POINT('',(32.5,-19.4,5.)) ;
#3115 = CARTESIAN_POINT('',(32.5,-19.4,5.)) ;
#3116 = CARTESIAN_POINT('',(-32.5,-19.4,5.)) ;
#3117 = CARTESIAN_POINT('',(32.5,-19.4,5.)) ;
#3118 = CARTESIAN_POINT('',(-32.5,-19.4,5.)) ;
#3119 = CARTESIAN_POINT('Origin',(32.5,-19.4,5.)) ;
#3120 = CARTESIAN_POINT('',(32.5,19.4,1.9)) ;
#3121 = CARTESIAN_POINT('',(32.5,-19.4,1.9)) ;
#3122 = CARTESIAN_POINT('',(32.5,19.4,5.)) ;
#3123 = CARTESIAN_POINT('',(32.5,19.4,5.)) ;
#3124 = CARTESIAN_POINT('',(32.5,-19.4,5.)) ;
#3125 = CARTESIAN_POINT('Origin',(32.5,19.4,5.)) ;
#3126 = CARTESIAN_POINT('',(-32.5,19.4,1.9)) ;
#3127 = CARTESIAN_POINT('',(32.5,19.4,1.9)) ;
#3128 = CARTESIAN_POINT('',(-32.5,19.4,5.)) ;
#3129 = CARTESIAN_POINT('',(-32.5,19.4,5.)) ;
#3130 = CARTESIAN_POINT('',(32.5,19.4,5.)) ;
#3131 = CARTESIAN_POINT('Origin',(-32.5,-19.4,5.)) ;
#3132 = CARTESIAN_POINT('',(-32.5,-19.4,1.9)) ;
#3133 = CARTESIAN_POINT('',(-32.5,-19.4,5.)) ;
#3134 = CARTESIAN_POINT('Origin',(0.,0.,5.)) ;
#3135 = CARTESIAN_POINT('',(-24.6,16.2,5.)) ;
#3136 = CARTESIAN_POINT('',(3.4,16.2,5.)) ;
#3137 = CARTESIAN_POINT('',(0.,16.2,5.)) ;
#3138 = CARTESIAN_POINT('',(3.4,4.20000000000001,5.)) ;
#3139 = CARTESIAN_POINT('',(3.4,0.,5.)) ;
#3140 = CARTESIAN_POINT('',(-24.6,4.20000000000001,5.)) ;
#3141 = CARTESIAN_POINT('',(3.12250225675826E-16,4.20000000000001,5.)) ;
#3142 = CARTESIAN_POINT('',(-24.6,0.,5.)) ;
#3143 = CARTESIAN_POINT('',(-28.1,-3.29999999999999,5.)) ;
#3144 = CARTESIAN_POINT('',(6.90000000000001,-3.29999999999999,5.)) ;
#3145 = CARTESIAN_POINT('',(-3.92543140849608E-16,-3.29999999999999,5.)) ;
#3146 = CARTESIAN_POINT('',(6.90000000000001,-18.3,5.)) ;
#3147 = CARTESIAN_POINT('',(6.90000000000001,0.,5.)) ;
#3148 = CARTESIAN_POINT('',(-28.1,-18.3,5.)) ;
#3149 = CARTESIAN_POINT('',(0.,-18.3,5.)) ;
#3150 = CARTESIAN_POINT('',(-28.1,0.,5.)) ;
#3151 = CARTESIAN_POINT('Origin',(34.9,-21.8,1.9)) ;
#3152 = CARTESIAN_POINT('',(34.9,-21.6,1.9)) ;
#3153 = CARTESIAN_POINT('',(34.9,21.6,1.9)) ;
#3154 = CARTESIAN_POINT('',(34.9,-21.8,1.9)) ;
#3155 = CARTESIAN_POINT('',(34.9,-21.6,0.)) ;
#3156 = CARTESIAN_POINT('',(34.9,-21.6,0.)) ;
#3157 = CARTESIAN_POINT('',(34.9,21.6,0.)) ;
#3158 = CARTESIAN_POINT('',(34.9,-21.8,0.)) ;
#3159 = CARTESIAN_POINT('',(34.9,21.6,1.9)) ;
#3160 = CARTESIAN_POINT('Origin',(34.9,21.8,1.9)) ;
#3161 = CARTESIAN_POINT('',(34.7,21.8,0.)) ;
#3162 = CARTESIAN_POINT('',(-34.7,21.8,0.)) ;
#3163 = CARTESIAN_POINT('',(34.9,21.8,0.)) ;
#3164 = CARTESIAN_POINT('',(-34.7,21.8,1.9)) ;
#3165 = CARTESIAN_POINT('',(-34.7,21.8,1.9)) ;
#3166 = CARTESIAN_POINT('',(34.7,21.8,1.9)) ;
#3167 = CARTESIAN_POINT('',(34.9,21.8,1.9)) ;
#3168 = CARTESIAN_POINT('',(34.7,21.8,1.9)) ;
#3169 = CARTESIAN_POINT('Origin',(-34.9,-21.8,1.9)) ;
#3170 = CARTESIAN_POINT('',(-34.9,-21.6,0.)) ;
#3171 = CARTESIAN_POINT('',(-34.9,21.6,0.)) ;
#3172 = CARTESIAN_POINT('',(-34.9,-21.8,0.)) ;
#3173 = CARTESIAN_POINT('',(-34.9,-21.6,1.9)) ;
#3174 = CARTESIAN_POINT('',(-34.9,-21.6,1.9)) ;
#3175 = CARTESIAN_POINT('',(-34.9,21.6,1.9)) ;
#3176 = CARTESIAN_POINT('',(-34.9,-21.8,1.9)) ;
#3177 = CARTESIAN_POINT('',(-34.9,21.6,0.)) ;
#3178 = CARTESIAN_POINT('Origin',(34.9,-21.8,1.9)) ;
#3179 = CARTESIAN_POINT('',(34.7,-21.8,0.)) ;
#3180 = CARTESIAN_POINT('',(-34.7,-21.8,0.)) ;
#3181 = CARTESIAN_POINT('',(34.9,-21.8,0.)) ;
#3182 = CARTESIAN_POINT('',(34.7,-21.8,1.9)) ;
#3183 = CARTESIAN_POINT('',(34.7,-21.8,1.9)) ;
#3184 = CARTESIAN_POINT('',(-34.7,-21.8,1.9)) ;
#3185 = CARTESIAN_POINT('',(34.9,-21.8,1.9)) ;
#3186 = CARTESIAN_POINT('',(-34.7,-21.8,1.9)) ;
#3187 = CARTESIAN_POINT('Origin',(0.,0.,1.9)) ;
#3188 = CARTESIAN_POINT('Origin',(34.7,-21.6,1.9)) ;
#3189 = CARTESIAN_POINT('Origin',(34.7,21.6,1.9)) ;
#3190 = CARTESIAN_POINT('Origin',(-34.7,21.6,1.9)) ;
#3191 = CARTESIAN_POINT('Origin',(-34.7,-21.6,1.9)) ;
#3192 = CARTESIAN_POINT('Origin',(0.,0.,0.)) ;
#3193 = CARTESIAN_POINT('Origin',(34.7,-21.6,0.)) ;
#3194 = CARTESIAN_POINT('Origin',(-34.7,-21.6,0.)) ;
#3195 = CARTESIAN_POINT('Origin',(-34.7,21.6,0.)) ;
#3196 = CARTESIAN_POINT('Origin',(34.7,21.6,0.)) ;
#3197 = CARTESIAN_POINT('',(3.4,16.2,0.)) ;
#3198 = CARTESIAN_POINT('',(3.4,4.20000000000001,0.)) ;
#3199 = CARTESIAN_POINT('',(3.4,4.20000000000001,0.)) ;
#3200 = CARTESIAN_POINT('',(-24.6,16.2,0.)) ;
#3201 = CARTESIAN_POINT('',(-24.6,16.2,0.)) ;
#3202 = CARTESIAN_POINT('',(-24.6,4.20000000000001,0.)) ;
#3203 = CARTESIAN_POINT('',(-24.6,4.20000000000001,0.)) ;
#3204 = CARTESIAN_POINT('',(-24.6,4.20000000000001,0.)) ;
#3205 = CARTESIAN_POINT('',(6.90000000000001,-3.29999999999999,0.)) ;
#3206 = CARTESIAN_POINT('',(6.90000000000001,-18.3,0.)) ;
#3207 = CARTESIAN_POINT('',(6.90000000000001,-18.3,0.)) ;
#3208 = CARTESIAN_POINT('',(-28.1,-3.29999999999999,0.)) ;
#3209 = CARTESIAN_POINT('',(-28.1,-3.29999999999999,0.)) ;
#3210 = CARTESIAN_POINT('',(-28.1,-18.3,0.)) ;
#3211 = CARTESIAN_POINT('',(-28.1,-18.3,0.)) ;
#3212 = CARTESIAN_POINT('',(-28.1,-18.3,0.)) ;
#3213 = CARTESIAN_POINT('Origin',(34.7,-21.6,1.9)) ;
#3214 = CARTESIAN_POINT('Origin',(-34.7,-21.6,1.9)) ;
#3215 = CARTESIAN_POINT('Origin',(-34.7,21.6,1.9)) ;
#3216 = CARTESIAN_POINT('Origin',(34.7,21.6,1.9)) ;
#3217 = CARTESIAN_POINT('Origin',(6.90000000000001,-18.3,6.)) ;
#3218 = CARTESIAN_POINT('',(6.90000000000001,-3.29999999999999,6.)) ;
#3219 = CARTESIAN_POINT('',(6.90000000000001,-18.3,6.)) ;
#3220 = CARTESIAN_POINT('Origin',(-28.1,-3.29999999999999,6.)) ;
#3221 = CARTESIAN_POINT('',(-28.1,-3.29999999999999,6.)) ;
#3222 = CARTESIAN_POINT('Origin',(-28.1,-18.3,6.)) ;
#3223 = CARTESIAN_POINT('',(-28.1,-18.3,6.)) ;
#3224 = CARTESIAN_POINT('Origin',(-28.1,-18.3,6.)) ;
#3225 = CARTESIAN_POINT('Origin',(3.4,4.20000000000001,6.)) ;
#3226 = CARTESIAN_POINT('',(3.4,16.2,6.)) ;
#3227 = CARTESIAN_POINT('',(3.4,4.20000000000001,6.)) ;
#3228 = CARTESIAN_POINT('Origin',(-24.6,16.2,6.)) ;
#3229 = CARTESIAN_POINT('',(-24.6,16.2,6.)) ;
#3230 = CARTESIAN_POINT('Origin',(-24.6,4.20000000000001,6.)) ;
#3231 = CARTESIAN_POINT('',(-24.6,4.20000000000001,6.)) ;
#3232 = CARTESIAN_POINT('Origin',(-24.6,4.20000000000001,6.)) ;
#3233 = CARTESIAN_POINT('',(0.,0.,0.)) ;
#3234 = CARTESIAN_POINT('Origin',(52.5,-19.4,5.)) ;
#3235 = CARTESIAN_POINT('',(52.5,-19.4,1.9)) ;
#3236 = CARTESIAN_POINT('',(-52.5,-19.4,1.9)) ;
#3237 = CARTESIAN_POINT('',(52.5,-19.4,1.9)) ;
#3238 = CARTESIAN_POINT('',(52.5,-19.4,5.)) ;
#3239 = CARTESIAN_POINT('',(52.5,-19.4,5.)) ;
#3240 = CARTESIAN_POINT('',(-52.5,-19.4,5.)) ;
#3241 = CARTESIAN_POINT('',(52.5,-19.4,5.)) ;
#3242 = CARTESIAN_POINT('',(-52.5,-19.4,5.)) ;
#3243 = CARTESIAN_POINT('Origin',(52.5,-19.4,5.)) ;
#3244 = CARTESIAN_POINT('',(52.5,19.4,1.9)) ;
#3245 = CARTESIAN_POINT('',(52.5,-19.4,1.9)) ;
#3246 = CARTESIAN_POINT('',(52.5,19.4,5.)) ;
#3247 = CARTESIAN_POINT('',(52.5,19.4,5.)) ;
#3248 = CARTESIAN_POINT('',(52.5,-19.4,5.)) ;
#3249 = CARTESIAN_POINT('Origin',(52.5,19.4,5.)) ;
#3250 = CARTESIAN_POINT('',(-52.5,19.4,1.9)) ;
#3251 = CARTESIAN_POINT('',(52.5,19.4,1.9)) ;
#3252 = CARTESIAN_POINT('',(-52.5,19.4,5.)) ;
#3253 = CARTESIAN_POINT('',(-52.5,19.4,5.)) ;
#3254 = CARTESIAN_POINT('',(52.5,19.4,5.)) ;
#3255 = CARTESIAN_POINT('Origin',(-52.5,-19.4,5.)) ;
#3256 = CARTESIAN_POINT('',(-52.5,-19.4,1.9)) ;
#3257 = CARTESIAN_POINT('',(-52.5,-19.4,5.)) ;
#3258 = CARTESIAN_POINT('Origin',(0.,0.,5.)) ;
#3259 = CARTESIAN_POINT('',(-4.6,6.00000000000001,5.)) ;
#3260 = CARTESIAN_POINT('',(23.4,6.00000000000001,5.)) ;
#3261 = CARTESIAN_POINT('',(7.43452918275775E-16,6.00000000000001,5.)) ;
#3262 = CARTESIAN_POINT('',(23.4,-6.,5.)) ;
#3263 = CARTESIAN_POINT('',(23.4,0.,5.)) ;
#3264 = CARTESIAN_POINT('',(-4.6,-5.99999999999999,5.)) ;
#3265 = CARTESIAN_POINT('',(-7.43452918275773E-16,-5.99999999999999,5.)) ;
#3266 = CARTESIAN_POINT('',(-4.6,0.,5.)) ;
#3267 = CARTESIAN_POINT('',(-17.1,-5.99999999999999,5.)) ;
#3268 = CARTESIAN_POINT('',(-45.1,-5.99999999999999,5.)) ;
#3269 = CARTESIAN_POINT('',(0.,-5.99999999999999,5.)) ;
#3270 = CARTESIAN_POINT('',(-45.1,6.00000000000001,5.)) ;
#3271 = CARTESIAN_POINT('',(-45.1,0.,5.)) ;
#3272 = CARTESIAN_POINT('',(-17.1,6.00000000000001,5.)) ;
#3273 = CARTESIAN_POINT('',(0.,6.00000000000001,5.)) ;
#3274 = CARTESIAN_POINT('',(-17.1,0.,5.)) ;
#3275 = CARTESIAN_POINT('Origin',(54.9,-21.8,1.9)) ;
#3276 = CARTESIAN_POINT('',(54.9,-21.6,1.9)) ;
#3277 = CARTESIAN_POINT('',(54.9,21.6,1.9)) ;
#3278 = CARTESIAN_POINT('',(54.9,-21.8,1.9)) ;
#3279 = CARTESIAN_POINT('',(54.9,-21.6,0.)) ;
#3280 = CARTESIAN_POINT('',(54.9,-21.6,0.)) ;
#3281 = CARTESIAN_POINT('',(54.9,21.6,0.)) ;
#3282 = CARTESIAN_POINT('',(54.9,-21.8,0.)) ;
#3283 = CARTESIAN_POINT('',(54.9,21.6,1.9)) ;
#3284 = CARTESIAN_POINT('Origin',(54.9,21.8,1.9)) ;
#3285 = CARTESIAN_POINT('',(54.7,21.8,0.)) ;
#3286 = CARTESIAN_POINT('',(-54.7,21.8,0.)) ;
#3287 = CARTESIAN_POINT('',(54.9,21.8,0.)) ;
#3288 = CARTESIAN_POINT('',(-54.7,21.8,1.9)) ;
#3289 = CARTESIAN_POINT('',(-54.7,21.8,1.9)) ;
#3290 = CARTESIAN_POINT('',(54.7,21.8,1.9)) ;
#3291 = CARTESIAN_POINT('',(54.9,21.8,1.9)) ;
#3292 = CARTESIAN_POINT('',(54.7,21.8,1.9)) ;
#3293 = CARTESIAN_POINT('Origin',(-54.9,-21.8,1.9)) ;
#3294 = CARTESIAN_POINT('',(-54.9,-21.6,0.)) ;
#3295 = CARTESIAN_POINT('',(-54.9,21.6,0.)) ;
#3296 = CARTESIAN_POINT('',(-54.9,-21.8,0.)) ;
#3297 = CARTESIAN_POINT('',(-54.9,-21.6,1.9)) ;
#3298 = CARTESIAN_POINT('',(-54.9,-21.6,1.9)) ;
#3299 = CARTESIAN_POINT('',(-54.9,21.6,1.9)) ;
#3300 = CARTESIAN_POINT('',(-54.9,-21.8,1.9)) ;
#3301 = CARTESIAN_POINT('',(-54.9,21.6,0.)) ;
#3302 = CARTESIAN_POINT('Origin',(54.9,-21.8,1.9)) ;
#3303 = CARTESIAN_POINT('',(54.7,-21.8,0.)) ;
#3304 = CARTESIAN_POINT('',(-54.7,-21.8,0.)) ;
#3305 = CARTESIAN_POINT('',(54.9,-21.8,0.)) ;
#3306 = CARTESIAN_POINT('',(54.7,-21.8,1.9)) ;
#3307 = CARTESIAN_POINT('',(54.7,-21.8,1.9)) ;
#3308 = CARTESIAN_POINT('',(-54.7,-21.8,1.9)) ;
#3309 = CARTESIAN_POINT('',(54.9,-21.8,1.9)) ;
#3310 = CARTESIAN_POINT('',(-54.7,-21.8,1.9)) ;
#3311 = CARTESIAN_POINT('Origin',(0.,0.,1.9)) ;
#3312 = CARTESIAN_POINT('Origin',(54.7,-21.6,1.9)) ;
#3313 = CARTESIAN_POINT('Origin',(54.7,21.6,1.9)) ;
#3314 = CARTESIAN_POINT('Origin',(-54.7,21.6,1.9)) ;
#3315 = CARTESIAN_POINT('Origin',(-54.7,-21.6,1.9)) ;
#3316 = CARTESIAN_POINT('Origin',(0.,0.,0.)) ;
#3317 = CARTESIAN_POINT('Origin',(54.7,-21.6,0.)) ;
#3318 = CARTESIAN_POINT('Origin',(-54.7,-21.6,0.)) ;
#3319 = CARTESIAN_POINT('Origin',(-54.7,21.6,0.)) ;
#3320 = CARTESIAN_POINT('Origin',(54.7,21.6,0.)) ;
#3321 = CARTESIAN_POINT('',(23.4,6.00000000000001,0.)) ;
#3322 = CARTESIAN_POINT('',(23.4,-6.,0.)) ;
#3323 = CARTESIAN_POINT('',(23.4,-6.,0.)) ;
#3324 = CARTESIAN_POINT('',(-4.6,6.00000000000001,0.)) ;
#3325 = CARTESIAN_POINT('',(-4.6,6.00000000000001,0.)) ;
#3326 = CARTESIAN_POINT('',(-4.6,-5.99999999999999,0.)) ;
#3327 = CARTESIAN_POINT('',(-4.6,-5.99999999999999,0.)) ;
#3328 = CARTESIAN_POINT('',(-4.6,-5.99999999999999,0.)) ;
#3329 = CARTESIAN_POINT('',(-45.1,-5.99999999999999,0.)) ;
#3330 = CARTESIAN_POINT('',(-45.1,6.00000000000001,0.)) ;
#3331 = CARTESIAN_POINT('',(-45.1,-5.99999999999999,0.)) ;
#3332 = CARTESIAN_POINT('',(-17.1,-5.99999999999999,0.)) ;
#3333 = CARTESIAN_POINT('',(-17.1,-5.99999999999999,0.)) ;
#3334 = CARTESIAN_POINT('',(-17.1,6.00000000000001,0.)) ;
#3335 = CARTESIAN_POINT('',(-17.1,-5.99999999999999,0.)) ;
#3336 = CARTESIAN_POINT('',(-17.1,6.00000000000001,0.)) ;
#3337 = CARTESIAN_POINT('Origin',(54.7,-21.6,1.9)) ;
#3338 = CARTESIAN_POINT('Origin',(-54.7,-21.6,1.9)) ;
#3339 = CARTESIAN_POINT('Origin',(-54.7,21.6,1.9)) ;
#3340 = CARTESIAN_POINT('Origin',(54.7,21.6,1.9)) ;
#3341 = CARTESIAN_POINT('Origin',(-45.1,-5.99999999999999,6.)) ;
#3342 = CARTESIAN_POINT('',(-45.1,-5.99999999999999,6.)) ;
#3343 = CARTESIAN_POINT('',(-45.1,6.00000000000001,6.)) ;
#3344 = CARTESIAN_POINT('Origin',(-17.1,-5.99999999999999,6.)) ;
#3345 = CARTESIAN_POINT('',(-17.1,-5.99999999999999,6.)) ;
#3346 = CARTESIAN_POINT('Origin',(-17.1,-5.99999999999999,6.)) ;
#3347 = CARTESIAN_POINT('',(-17.1,6.00000000000001,6.)) ;
#3348 = CARTESIAN_POINT('Origin',(-17.1,6.00000000000001,6.)) ;
#3349 = CARTESIAN_POINT('Origin',(23.4,-6.,6.)) ;
#3350 = CARTESIAN_POINT('',(23.4,6.00000000000001,6.)) ;
#3351 = CARTESIAN_POINT('',(23.4,-6.,6.)) ;
#3352 = CARTESIAN_POINT('Origin',(-4.6,6.00000000000001,6.)) ;
#3353 = CARTESIAN_POINT('',(-4.6,6.00000000000001,6.)) ;
#3354 = CARTESIAN_POINT('Origin',(-4.6,-5.99999999999999,6.)) ;
#3355 = CARTESIAN_POINT('',(-4.6,-5.99999999999999,6.)) ;
#3356 = CARTESIAN_POINT('Origin',(-4.6,-5.99999999999999,6.)) ;
#3357 = CARTESIAN_POINT('',(0.,0.,0.)) ;
#3358 = CARTESIAN_POINT('Origin',(52.5,-19.4,5.)) ;
#3359 = CARTESIAN_POINT('',(52.5,-19.4,1.9)) ;
#3360 = CARTESIAN_POINT('',(-52.5,-19.4,1.9)) ;
#3361 = CARTESIAN_POINT('',(52.5,-19.4,1.9)) ;
#3362 = CARTESIAN_POINT('',(52.5,-19.4,5.)) ;
#3363 = CARTESIAN_POINT('',(52.5,-19.4,5.)) ;
#3364 = CARTESIAN_POINT('',(-52.5,-19.4,5.)) ;
#3365 = CARTESIAN_POINT('',(52.5,-19.4,5.)) ;
#3366 = CARTESIAN_POINT('',(-52.5,-19.4,5.)) ;
#3367 = CARTESIAN_POINT('Origin',(52.5,-19.4,5.)) ;
#3368 = CARTESIAN_POINT('',(52.5,19.4,1.9)) ;
#3369 = CARTESIAN_POINT('',(52.5,-19.4,1.9)) ;
#3370 = CARTESIAN_POINT('',(52.5,19.4,5.)) ;
#3371 = CARTESIAN_POINT('',(52.5,19.4,5.)) ;
#3372 = CARTESIAN_POINT('',(52.5,-19.4,5.)) ;
#3373 = CARTESIAN_POINT('Origin',(52.5,19.4,5.)) ;
#3374 = CARTESIAN_POINT('',(-52.5,19.4,1.9)) ;
#3375 = CARTESIAN_POINT('',(52.5,19.4,1.9)) ;
#3376 = CARTESIAN_POINT('',(-52.5,19.4,5.)) ;
#3377 = CARTESIAN_POINT('',(-52.5,19.4,5.)) ;
#3378 = CARTESIAN_POINT('',(52.5,19.4,5.)) ;
#3379 = CARTESIAN_POINT('Origin',(-52.5,-19.4,5.)) ;
#3380 = CARTESIAN_POINT('',(-52.5,-19.4,1.9)) ;
#3381 = CARTESIAN_POINT('',(-52.5,-19.4,5.)) ;
#3382 = CARTESIAN_POINT('Origin',(0.,0.,5.)) ;
#3383 = CARTESIAN_POINT('',(6.1,10.5,5.)) ;
#3384 = CARTESIAN_POINT('',(34.1,10.5,5.)) ;
#3385 = CARTESIAN_POINT('',(1.04083408558609E-15,10.5,5.)) ;
#3386 = CARTESIAN_POINT('',(34.1,-1.5,5.)) ;
#3387 = CARTESIAN_POINT('',(34.1,0.,5.)) ;
#3388 = CARTESIAN_POINT('',(6.1,-1.49999999999999,5.)) ;
#3389 = CARTESIAN_POINT('',(-2.23035875482731E-16,-1.49999999999999,5.)) ;
#3390 = CARTESIAN_POINT('',(6.1,0.,5.)) ;
#3391 = CARTESIAN_POINT('Origin',(54.9,-21.8,1.9)) ;
#3392 = CARTESIAN_POINT('',(54.9,-21.6,1.9)) ;
#3393 = CARTESIAN_POINT('',(54.9,21.6,1.9)) ;
#3394 = CARTESIAN_POINT('',(54.9,-21.8,1.9)) ;
#3395 = CARTESIAN_POINT('',(54.9,-21.6,0.)) ;
#3396 = CARTESIAN_POINT('',(54.9,-21.6,0.)) ;
#3397 = CARTESIAN_POINT('',(54.9,21.6,0.)) ;
#3398 = CARTESIAN_POINT('',(54.9,-21.8,0.)) ;
#3399 = CARTESIAN_POINT('',(54.9,21.6,1.9)) ;
#3400 = CARTESIAN_POINT('Origin',(54.9,21.8,1.9)) ;
#3401 = CARTESIAN_POINT('',(54.7,21.8,0.)) ;
#3402 = CARTESIAN_POINT('',(-54.7,21.8,0.)) ;
#3403 = CARTESIAN_POINT('',(54.9,21.8,0.)) ;
#3404 = CARTESIAN_POINT('',(-54.7,21.8,1.9)) ;
#3405 = CARTESIAN_POINT('',(-54.7,21.8,1.9)) ;
#3406 = CARTESIAN_POINT('',(54.7,21.8,1.9)) ;
#3407 = CARTESIAN_POINT('',(54.9,21.8,1.9)) ;
#3408 = CARTESIAN_POINT('',(54.7,21.8,1.9)) ;
#3409 = CARTESIAN_POINT('Origin',(-54.9,-21.8,1.9)) ;
#3410 = CARTESIAN_POINT('',(-54.9,-21.6,0.)) ;
#3411 = CARTESIAN_POINT('',(-54.9,21.6,0.)) ;
#3412 = CARTESIAN_POINT('',(-54.9,-21.8,0.)) ;
#3413 = CARTESIAN_POINT('',(-54.9,-21.6,1.9)) ;
#3414 = CARTESIAN_POINT('',(-54.9,-21.6,1.9)) ;
#3415 = CARTESIAN_POINT('',(-54.9,21.6,1.9)) ;
#3416 = CARTESIAN_POINT('',(-54.9,-21.8,1.9)) ;
#3417 = CARTESIAN_POINT('',(-54.9,21.6,0.)) ;
#3418 = CARTESIAN_POINT('Origin',(54.9,-21.8,1.9)) ;
#3419 = CARTESIAN_POINT('',(54.7,-21.8,0.)) ;
#3420 = CARTESIAN_POINT('',(-54.7,-21.8,0.)) ;
#3421 = CARTESIAN_POINT('',(54.9,-21.8,0.)) ;
#3422 = CARTESIAN_POINT('',(54.7,-21.8,1.9)) ;
#3423 = CARTESIAN_POINT('',(54.7,-21.8,1.9)) ;
#3424 = CARTESIAN_POINT('',(-54.7,-21.8,1.9)) ;
#3425 = CARTESIAN_POINT('',(54.9,-21.8,1.9)) ;
#3426 = CARTESIAN_POINT('',(-54.7,-21.8,1.9)) ;
#3427 = CARTESIAN_POINT('Origin',(0.,0.,1.9)) ;
#3428 = CARTESIAN_POINT('Origin',(54.7,-21.6,1.9)) ;
#3429 = CARTESIAN_POINT('Origin',(54.7,21.6,1.9)) ;
#3430 = CARTESIAN_POINT('Origin',(-54.7,21.6,1.9)) ;
#3431 = CARTESIAN_POINT('Origin',(-54.7,-21.6,1.9)) ;
#3432 = CARTESIAN_POINT('Origin',(0.,0.,0.)) ;
#3433 = CARTESIAN_POINT('Origin',(54.7,-21.6,0.)) ;
#3434 = CARTESIAN_POINT('Origin',(-54.7,-21.6,0.)) ;
#3435 = CARTESIAN_POINT('Origin',(-54.7,21.6,0.)) ;
#3436 = CARTESIAN_POINT('Origin',(54.7,21.6,0.)) ;
#3437 = CARTESIAN_POINT('',(34.1,10.5,0.)) ;
#3438 = CARTESIAN_POINT('',(34.1,-1.5,0.)) ;
#3439 = CARTESIAN_POINT('',(34.1,-1.5,0.)) ;
#3440 = CARTESIAN_POINT('',(6.1,10.5,0.)) ;
#3441 = CARTESIAN_POINT('',(6.1,10.5,0.)) ;
#3442 = CARTESIAN_POINT('',(6.1,-1.49999999999999,0.)) ;
#3443 = CARTESIAN_POINT('',(6.1,-1.49999999999999,0.)) ;
#3444 = CARTESIAN_POINT('',(6.1,-1.49999999999999,0.)) ;
#3445 = CARTESIAN_POINT('Origin',(54.7,-21.6,1.9)) ;
#3446 = CARTESIAN_POINT('Origin',(-54.7,-21.6,1.9)) ;
#3447 = CARTESIAN_POINT('Origin',(-54.7,21.6,1.9)) ;
#3448 = CARTESIAN_POINT('Origin',(54.7,21.6,1.9)) ;
#3449 = CARTESIAN_POINT('Origin',(34.1,-1.5,6.)) ;
#3450 = CARTESIAN_POINT('',(34.1,10.5,6.)) ;
#3451 = CARTESIAN_POINT('',(34.1,-1.5,6.)) ;
#3452 = CARTESIAN_POINT('Origin',(6.1,10.5,6.)) ;
#3453 = CARTESIAN_POINT('',(6.1,10.5,6.)) ;
#3454 = CARTESIAN_POINT('Origin',(6.1,-1.49999999999999,6.)) ;
#3455 = CARTESIAN_POINT('',(6.1,-1.49999999999999,6.)) ;
#3456 = CARTESIAN_POINT('Origin',(6.1,-1.49999999999999,6.)) ;
#3457 = CARTESIAN_POINT('',(0.,0.,0.)) ;
#3458 = CARTESIAN_POINT('Origin',(52.5,-32.5,5.)) ;
#3459 = CARTESIAN_POINT('',(52.5,-32.5,1.9)) ;
#3460 = CARTESIAN_POINT('',(-52.5,-32.5,1.9)) ;
#3461 = CARTESIAN_POINT('',(52.5,-32.5,1.9)) ;
#3462 = CARTESIAN_POINT('',(52.5,-32.5,5.)) ;
#3463 = CARTESIAN_POINT('',(52.5,-32.5,5.)) ;
#3464 = CARTESIAN_POINT('',(-52.5,-32.5,5.)) ;
#3465 = CARTESIAN_POINT('',(52.5,-32.5,5.)) ;
#3466 = CARTESIAN_POINT('',(-52.5,-32.5,5.)) ;
#3467 = CARTESIAN_POINT('Origin',(52.5,-32.5,5.)) ;
#3468 = CARTESIAN_POINT('',(52.5,32.5,1.9)) ;
#3469 = CARTESIAN_POINT('',(52.5,-32.5,1.9)) ;
#3470 = CARTESIAN_POINT('',(52.5,32.5,5.)) ;
#3471 = CARTESIAN_POINT('',(52.5,32.5,5.)) ;
#3472 = CARTESIAN_POINT('',(52.5,-32.5,5.)) ;
#3473 = CARTESIAN_POINT('Origin',(52.5,32.5,5.)) ;
#3474 = CARTESIAN_POINT('',(-52.5,32.5,1.9)) ;
#3475 = CARTESIAN_POINT('',(52.5,32.5,1.9)) ;
#3476 = CARTESIAN_POINT('',(-52.5,32.5,5.)) ;
#3477 = CARTESIAN_POINT('',(-52.5,32.5,5.)) ;
#3478 = CARTESIAN_POINT('',(52.5,32.5,5.)) ;
#3479 = CARTESIAN_POINT('Origin',(-52.5,-32.5,5.)) ;
#3480 = CARTESIAN_POINT('',(-52.5,-32.5,1.9)) ;
#3481 = CARTESIAN_POINT('',(-52.5,-32.5,5.)) ;
#3482 = CARTESIAN_POINT('Origin',(0.,0.,5.)) ;
#3483 = CARTESIAN_POINT('Origin',(54.9,-34.9,1.9)) ;
#3484 = CARTESIAN_POINT('',(54.9,-34.7,1.9)) ;
#3485 = CARTESIAN_POINT('',(54.9,34.7,1.9)) ;
#3486 = CARTESIAN_POINT('',(54.9,-34.9,1.9)) ;
#3487 = CARTESIAN_POINT('',(54.9,-34.7,0.)) ;
#3488 = CARTESIAN_POINT('',(54.9,-34.7,0.)) ;
#3489 = CARTESIAN_POINT('',(54.9,34.7,0.)) ;
#3490 = CARTESIAN_POINT('',(54.9,-34.9,0.)) ;
#3491 = CARTESIAN_POINT('',(54.9,34.7,1.9)) ;
#3492 = CARTESIAN_POINT('Origin',(54.9,34.9,1.9)) ;
#3493 = CARTESIAN_POINT('',(54.7,34.9,0.)) ;
#3494 = CARTESIAN_POINT('',(-54.7,34.9,0.)) ;
#3495 = CARTESIAN_POINT('',(54.9,34.9,0.)) ;
#3496 = CARTESIAN_POINT('',(-54.7,34.9,1.9)) ;
#3497 = CARTESIAN_POINT('',(-54.7,34.9,1.9)) ;
#3498 = CARTESIAN_POINT('',(54.7,34.9,1.9)) ;
#3499 = CARTESIAN_POINT('',(54.9,34.9,1.9)) ;
#3500 = CARTESIAN_POINT('',(54.7,34.9,1.9)) ;
#3501 = CARTESIAN_POINT('Origin',(-54.9,-34.9,1.9)) ;
#3502 = CARTESIAN_POINT('',(-54.9,-34.7,0.)) ;
#3503 = CARTESIAN_POINT('',(-54.9,34.7,0.)) ;
#3504 = CARTESIAN_POINT('',(-54.9,-34.9,0.)) ;
#3505 = CARTESIAN_POINT('',(-54.9,-34.7,1.9)) ;
#3506 = CARTESIAN_POINT('',(-54.9,-34.7,1.9)) ;
#3507 = CARTESIAN_POINT('',(-54.9,34.7,1.9)) ;
#3508 = CARTESIAN_POINT('',(-54.9,-34.9,1.9)) ;
#3509 = CARTESIAN_POINT('',(-54.9,34.7,0.)) ;
#3510 = CARTESIAN_POINT('Origin',(54.9,-34.9,1.9)) ;
#3511 = CARTESIAN_POINT('',(54.7,-34.9,0.)) ;
#3512 = CARTESIAN_POINT('',(-54.7,-34.9,0.)) ;
#3513 = CARTESIAN_POINT('',(54.9,-34.9,0.)) ;
#3514 = CARTESIAN_POINT('',(54.7,-34.9,1.9)) ;
#3515 = CARTESIAN_POINT('',(54.7,-34.9,1.9)) ;
#3516 = CARTESIAN_POINT('',(-54.7,-34.9,1.9)) ;
#3517 = CARTESIAN_POINT('',(54.9,-34.9,1.9)) ;
#3518 = CARTESIAN_POINT('',(-54.7,-34.9,1.9)) ;
#3519 = CARTESIAN_POINT('Origin',(0.,0.,1.9)) ;
#3520 = CARTESIAN_POINT('Origin',(54.7,-34.7,1.9)) ;
#3521 = CARTESIAN_POINT('Origin',(54.7,34.7,1.9)) ;
#3522 = CARTESIAN_POINT('Origin',(-54.7,34.7,1.9)) ;
#3523 = CARTESIAN_POINT('Origin',(-54.7,-34.7,1.9)) ;
#3524 = CARTESIAN_POINT('Origin',(0.,0.,0.)) ;
#3525 = CARTESIAN_POINT('Origin',(54.7,-34.7,0.)) ;
#3526 = CARTESIAN_POINT('Origin',(-54.7,-34.7,0.)) ;
#3527 = CARTESIAN_POINT('Origin',(-54.7,34.7,0.)) ;
#3528 = CARTESIAN_POINT('Origin',(54.7,34.7,0.)) ;
#3529 = CARTESIAN_POINT('Origin',(54.7,-34.7,1.9)) ;
#3530 = CARTESIAN_POINT('Origin',(-54.7,-34.7,1.9)) ;
#3531 = CARTESIAN_POINT('Origin',(-54.7,34.7,1.9)) ;
#3532 = CARTESIAN_POINT('Origin',(54.7,34.7,1.9)) ;
#3533 = CARTESIAN_POINT('',(0.,0.,0.)) ;
#3534 = CARTESIAN_POINT('Origin',(17.7,7.5,7.)) ;
#3535 = CARTESIAN_POINT('',(17.7,-7.7,6.8)) ;
#3536 = CARTESIAN_POINT('',(17.7,7.7,6.8)) ;
#3537 = CARTESIAN_POINT('',(17.7,7.5,6.8)) ;
#3538 = CARTESIAN_POINT('',(17.7,-7.7,0.2)) ;
#3539 = CARTESIAN_POINT('',(17.7,-7.7,7.)) ;
#3540 = CARTESIAN_POINT('',(17.7,7.7,0.2)) ;
#3541 = CARTESIAN_POINT('',(17.7,6.55031584528842E-15,0.2)) ;
#3542 = CARTESIAN_POINT('',(17.7,7.7,7.)) ;
#3543 = CARTESIAN_POINT('Origin',(-17.5,7.7,7.)) ;
#3544 = CARTESIAN_POINT('',(-17.7,7.7,6.8)) ;
#3545 = CARTESIAN_POINT('',(-17.5,7.7,6.8)) ;
#3546 = CARTESIAN_POINT('',(-17.7,7.7,0.2)) ;
#3547 = CARTESIAN_POINT('',(0.,7.7,0.2)) ;
#3548 = CARTESIAN_POINT('',(-17.7,7.7,7.)) ;
#3549 = CARTESIAN_POINT('Origin',(-17.7,7.5,7.)) ;
#3550 = CARTESIAN_POINT('',(-17.7,-7.7,6.8)) ;
#3551 = CARTESIAN_POINT('',(-17.7,7.5,6.8)) ;
#3552 = CARTESIAN_POINT('',(-17.7,-7.7,0.2)) ;
#3553 = CARTESIAN_POINT('',(-17.7,-6.55031584528843E-15,0.2)) ;
#3554 = CARTESIAN_POINT('',(-17.7,-7.7,7.)) ;
#3555 = CARTESIAN_POINT('Origin',(-17.5,-7.7,7.)) ;
#3556 = CARTESIAN_POINT('',(-17.5,-7.7,6.8)) ;
#3557 = CARTESIAN_POINT('',(0.,-7.7,0.2)) ;
#3558 = CARTESIAN_POINT('Origin',(0.,0.,0.2)) ;
#3559 = CARTESIAN_POINT('',(20.5,-10.5,0.2)) ;
#3560 = CARTESIAN_POINT('',(20.5,10.5,0.2)) ;
#3561 = CARTESIAN_POINT('',(20.5,7.5,0.2)) ;
#3562 = CARTESIAN_POINT('',(-20.5,10.5,0.2)) ;
#3563 = CARTESIAN_POINT('',(-17.5,10.5,0.2)) ;
#3564 = CARTESIAN_POINT('',(-20.5,-10.5,0.2)) ;
#3565 = CARTESIAN_POINT('',(-20.5,7.5,0.2)) ;
#3566 = CARTESIAN_POINT('',(-17.5,-10.5,0.2)) ;
#3567 = CARTESIAN_POINT('Origin',(0.,0.,0.)) ;
#3568 = CARTESIAN_POINT('',(20.5,-10.5,0.)) ;
#3569 = CARTESIAN_POINT('',(20.5,10.5,0.)) ;
#3570 = CARTESIAN_POINT('',(20.5,7.5,0.)) ;
#3571 = CARTESIAN_POINT('',(-20.5,-10.5,0.)) ;
#3572 = CARTESIAN_POINT('',(-17.5,-10.5,0.)) ;
#3573 = CARTESIAN_POINT('',(-20.5,10.5,0.)) ;
#3574 = CARTESIAN_POINT('',(-20.5,7.5,0.)) ;
#3575 = CARTESIAN_POINT('',(-17.5,10.5,0.)) ;
#3576 = CARTESIAN_POINT('',(17.5,-7.5,0.)) ;
#3577 = CARTESIAN_POINT('',(17.5,7.5,0.)) ;
#3578 = CARTESIAN_POINT('',(17.5,7.5,0.)) ;
#3579 = CARTESIAN_POINT('',(-17.5,7.5,0.)) ;
#3580 = CARTESIAN_POINT('',(-17.5,7.5,0.)) ;
#3581 = CARTESIAN_POINT('',(-17.5,-7.5,0.)) ;
#3582 = CARTESIAN_POINT('',(-17.5,7.5,0.)) ;
#3583 = CARTESIAN_POINT('',(-17.5,-7.5,0.)) ;
#3584 = CARTESIAN_POINT('Origin',(20.5,7.5,0.2)) ;
#3585 = CARTESIAN_POINT('',(20.5,10.5,0.2)) ;
#3586 = CARTESIAN_POINT('',(20.5,-10.5,0.2)) ;
#3587 = CARTESIAN_POINT('Origin',(-17.5,10.5,0.2)) ;
#3588 = CARTESIAN_POINT('',(-20.5,10.5,0.2)) ;
#3589 = CARTESIAN_POINT('Origin',(-20.5,7.5,0.2)) ;
#3590 = CARTESIAN_POINT('',(-20.5,-10.5,0.2)) ;
#3591 = CARTESIAN_POINT('Origin',(-17.5,-10.5,0.2)) ;
#3592 = CARTESIAN_POINT('Origin',(17.5,7.5,0.2)) ;
#3593 = CARTESIAN_POINT('',(17.5,7.5,7.)) ;
#3594 = CARTESIAN_POINT('',(17.5,7.5,0.2)) ;
#3595 = CARTESIAN_POINT('',(17.5,-7.5,7.)) ;
#3596 = CARTESIAN_POINT('',(17.5,-7.5,0.2)) ;
#3597 = CARTESIAN_POINT('',(17.5,7.5,7.)) ;
#3598 = CARTESIAN_POINT('Origin',(-17.5,7.5,0.2)) ;
#3599 = CARTESIAN_POINT('',(-17.5,7.5,7.)) ;
#3600 = CARTESIAN_POINT('',(-17.5,7.5,0.2)) ;
#3601 = CARTESIAN_POINT('',(-17.5,7.5,7.)) ;
#3602 = CARTESIAN_POINT('Origin',(-17.5,7.5,0.2)) ;
#3603 = CARTESIAN_POINT('',(-17.5,-7.5,7.)) ;
#3604 = CARTESIAN_POINT('',(-17.5,-7.5,0.2)) ;
#3605 = CARTESIAN_POINT('',(-17.5,7.5,7.)) ;
#3606 = CARTESIAN_POINT('Origin',(-17.5,-7.5,0.2)) ;
#3607 = CARTESIAN_POINT('',(-17.5,-7.5,7.)) ;
#3608 = CARTESIAN_POINT('Origin',(0.,0.,7.)) ;
#3609 = CARTESIAN_POINT('',(-20.5,10.5,7.)) ;
#3610 = CARTESIAN_POINT('',(-20.5,-10.5,7.)) ;
#3611 = CARTESIAN_POINT('',(-20.5,7.5,7.)) ;
#3612 = CARTESIAN_POINT('',(20.5,-10.5,7.)) ;
#3613 = CARTESIAN_POINT('',(-17.5,-10.5,7.)) ;
#3614 = CARTESIAN_POINT('',(20.5,10.5,7.)) ;
#3615 = CARTESIAN_POINT('',(20.5,-7.5,7.)) ;
#3616 = CARTESIAN_POINT('',(17.5,10.5,7.)) ;
#3617 = CARTESIAN_POINT('Origin',(0.,0.,6.8)) ;
#3618 = CARTESIAN_POINT('',(-20.5,10.5,6.8)) ;
#3619 = CARTESIAN_POINT('',(-20.5,-10.5,6.8)) ;
#3620 = CARTESIAN_POINT('',(-20.5,7.5,6.8)) ;
#3621 = CARTESIAN_POINT('',(20.5,10.5,6.8)) ;
#3622 = CARTESIAN_POINT('',(17.5,10.5,6.8)) ;
#3623 = CARTESIAN_POINT('',(20.5,-10.5,6.8)) ;
#3624 = CARTESIAN_POINT('',(20.5,-7.5,6.8)) ;
#3625 = CARTESIAN_POINT('',(-17.5,-10.5,6.8)) ;
#3626 = CARTESIAN_POINT('Origin',(-20.5,7.5,6.8)) ;
#3627 = CARTESIAN_POINT('',(-20.5,10.5,6.8)) ;
#3628 = CARTESIAN_POINT('',(-20.5,-10.5,6.8)) ;
#3629 = CARTESIAN_POINT('Origin',(17.5,10.5,6.8)) ;
#3630 = CARTESIAN_POINT('',(20.5,10.5,6.8)) ;
#3631 = CARTESIAN_POINT('Origin',(20.5,-7.5,6.8)) ;
#3632 = CARTESIAN_POINT('',(20.5,-10.5,6.8)) ;
#3633 = CARTESIAN_POINT('Origin',(-17.5,-10.5,6.8)) ;
#3634 = CARTESIAN_POINT('',(0.,0.,0.)) ;
#3635 = CARTESIAN_POINT('Origin',(14.2,6.,7.)) ;
#3636 = CARTESIAN_POINT('',(14.2,-6.2,6.8)) ;
#3637 = CARTESIAN_POINT('',(14.2,6.2,6.8)) ;
#3638 = CARTESIAN_POINT('',(14.2,6.,6.8)) ;
#3639 = CARTESIAN_POINT('',(14.2,-6.2,0.2)) ;
#3640 = CARTESIAN_POINT('',(14.2,-6.2,7.)) ;
#3641 = CARTESIAN_POINT('',(14.2,6.2,0.2)) ;
#3642 = CARTESIAN_POINT('',(14.2,-6.56881956236551E-15,0.2)) ;
#3643 = CARTESIAN_POINT('',(14.2,6.2,7.)) ;
#3644 = CARTESIAN_POINT('Origin',(-14.,6.2,7.)) ;
#3645 = CARTESIAN_POINT('',(-14.2,6.2,6.8)) ;
#3646 = CARTESIAN_POINT('',(-14.,6.2,6.8)) ;
#3647 = CARTESIAN_POINT('',(-14.2,6.2,0.2)) ;
#3648 = CARTESIAN_POINT('',(0.,6.2,0.2)) ;
#3649 = CARTESIAN_POINT('',(-14.2,6.2,7.)) ;
#3650 = CARTESIAN_POINT('Origin',(-14.2,6.,7.)) ;
#3651 = CARTESIAN_POINT('',(-14.2,-6.2,6.8)) ;
#3652 = CARTESIAN_POINT('',(-14.2,6.,6.8)) ;
#3653 = CARTESIAN_POINT('',(-14.2,-6.2,0.2)) ;
#3654 = CARTESIAN_POINT('',(-14.2,6.56881956236551E-15,0.2)) ;
#3655 = CARTESIAN_POINT('',(-14.2,-6.2,7.)) ;
#3656 = CARTESIAN_POINT('Origin',(-14.,-6.2,7.)) ;
#3657 = CARTESIAN_POINT('',(-14.,-6.2,6.8)) ;
#3658 = CARTESIAN_POINT('',(0.,-6.2,0.2)) ;
#3659 = CARTESIAN_POINT('Origin',(0.,0.,0.2)) ;
#3660 = CARTESIAN_POINT('',(17.,-9.,0.2)) ;
#3661 = CARTESIAN_POINT('',(17.,9.,0.2)) ;
#3662 = CARTESIAN_POINT('',(17.,6.,0.2)) ;
#3663 = CARTESIAN_POINT('',(-17.,9.,0.2)) ;
#3664 = CARTESIAN_POINT('',(-14.,9.,0.2)) ;
#3665 = CARTESIAN_POINT('',(-17.,-9.,0.2)) ;
#3666 = CARTESIAN_POINT('',(-17.,6.,0.2)) ;
#3667 = CARTESIAN_POINT('',(-14.,-9.,0.2)) ;
#3668 = CARTESIAN_POINT('Origin',(0.,0.,0.)) ;
#3669 = CARTESIAN_POINT('',(17.,-9.,0.)) ;
#3670 = CARTESIAN_POINT('',(17.,9.,0.)) ;
#3671 = CARTESIAN_POINT('',(17.,6.,0.)) ;
#3672 = CARTESIAN_POINT('',(-17.,-9.,0.)) ;
#3673 = CARTESIAN_POINT('',(-14.,-9.,0.)) ;
#3674 = CARTESIAN_POINT('',(-17.,9.,0.)) ;
#3675 = CARTESIAN_POINT('',(-17.,6.,0.)) ;
#3676 = CARTESIAN_POINT('',(-14.,9.,0.)) ;
#3677 = CARTESIAN_POINT('',(14.,-6.,0.)) ;
#3678 = CARTESIAN_POINT('',(14.,6.,0.)) ;
#3679 = CARTESIAN_POINT('',(14.,6.,0.)) ;
#3680 = CARTESIAN_POINT('',(-14.,6.,0.)) ;
#3681 = CARTESIAN_POINT('',(-14.,6.,0.)) ;
#3682 = CARTESIAN_POINT('',(-14.,-6.,0.)) ;
#3683 = CARTESIAN_POINT('',(-14.,6.,0.)) ;
#3684 = CARTESIAN_POINT('',(-14.,-6.,0.)) ;
#3685 = CARTESIAN_POINT('Origin',(17.,6.,0.2)) ;
#3686 = CARTESIAN_POINT('',(17.,9.,0.2)) ;
#3687 = CARTESIAN_POINT('',(17.,-9.,0.2)) ;
#3688 = CARTESIAN_POINT('Origin',(-14.,9.,0.2)) ;
#3689 = CARTESIAN_POINT('',(-17.,9.,0.2)) ;
#3690 = CARTESIAN_POINT('Origin',(-17.,6.,0.2)) ;
#3691 = CARTESIAN_POINT('',(-17.,-9.,0.2)) ;
#3692 = CARTESIAN_POINT('Origin',(-14.,-9.,0.2)) ;
#3693 = CARTESIAN_POINT('Origin',(14.,6.,0.2)) ;
#3694 = CARTESIAN_POINT('',(14.,6.,7.)) ;
#3695 = CARTESIAN_POINT('',(14.,6.,0.2)) ;
#3696 = CARTESIAN_POINT('',(14.,-6.,7.)) ;
#3697 = CARTESIAN_POINT('',(14.,-6.,0.2)) ;
#3698 = CARTESIAN_POINT('',(14.,6.,7.)) ;
#3699 = CARTESIAN_POINT('Origin',(-14.,6.,0.2)) ;
#3700 = CARTESIAN_POINT('',(-14.,6.,7.)) ;
#3701 = CARTESIAN_POINT('',(-14.,6.,0.2)) ;
#3702 = CARTESIAN_POINT('',(-14.,6.,7.)) ;
#3703 = CARTESIAN_POINT('Origin',(-14.,6.,0.2)) ;
#3704 = CARTESIAN_POINT('',(-14.,-6.,7.)) ;
#3705 = CARTESIAN_POINT('',(-14.,-6.,0.2)) ;
#3706 = CARTESIAN_POINT('',(-14.,6.,7.)) ;
#3707 = CARTESIAN_POINT('Origin',(-14.,-6.,0.2)) ;
#3708 = CARTESIAN_POINT('',(-14.,-6.,7.)) ;
#3709 = CARTESIAN_POINT('Origin',(0.,0.,7.)) ;
#3710 = CARTESIAN_POINT('',(-17.,9.,7.)) ;
#3711 = CARTESIAN_POINT('',(-17.,-9.,7.)) ;
#3712 = CARTESIAN_POINT('',(-17.,6.,7.)) ;
#3713 = CARTESIAN_POINT('',(17.,-9.,7.)) ;
#3714 = CARTESIAN_POINT('',(-14.,-9.,7.)) ;
#3715 = CARTESIAN_POINT('',(17.,9.,7.)) ;
#3716 = CARTESIAN_POINT('',(17.,-6.,7.)) ;
#3717 = CARTESIAN_POINT('',(14.,9.,7.)) ;
#3718 = CARTESIAN_POINT('Origin',(0.,0.,6.8)) ;
#3719 = CARTESIAN_POINT('',(-17.,9.,6.8)) ;
#3720 = CARTESIAN_POINT('',(-17.,-9.,6.8)) ;
#3721 = CARTESIAN_POINT('',(-17.,6.,6.8)) ;
#3722 = CARTESIAN_POINT('',(17.,9.,6.8)) ;
#3723 = CARTESIAN_POINT('',(14.,9.,6.8)) ;
#3724 = CARTESIAN_POINT('',(17.,-9.,6.8)) ;
#3725 = CARTESIAN_POINT('',(17.,-6.,6.8)) ;
#3726 = CARTESIAN_POINT('',(-14.,-9.,6.8)) ;
#3727 = CARTESIAN_POINT('Origin',(-17.,6.,6.8)) ;
#3728 = CARTESIAN_POINT('',(-17.,9.,6.8)) ;
#3729 = CARTESIAN_POINT('',(-17.,-9.,6.8)) ;
#3730 = CARTESIAN_POINT('Origin',(14.,9.,6.8)) ;
#3731 = CARTESIAN_POINT('',(17.,9.,6.8)) ;
#3732 = CARTESIAN_POINT('Origin',(17.,-6.,6.8)) ;
#3733 = CARTESIAN_POINT('',(17.,-9.,6.8)) ;
#3734 = CARTESIAN_POINT('Origin',(-14.,-9.,6.8)) ;
#3735 = CARTESIAN_POINT('',(120.331674233964,56.0679277164062,59.2432287417214)) ;
#3736 = CARTESIAN_POINT('',(82.7316742339655,56.0679277164065,1.64322874171421)) ;
#3737 = CARTESIAN_POINT('',(157.931674233965,56.0679277164062,1.6432287417133)) ;
#3738 = CARTESIAN_POINT('',(120.331674233964,80.5679277164065,1.64322874171967)) ;
#3739 = CARTESIAN_POINT('',(82.7316742339642,56.0679277164064,32.7432287417128)) ;
#3740 = CARTESIAN_POINT('',(130.931674233965,45.2679277164061,66.2432287417205)) ;
#3741 = CARTESIAN_POINT('',(82.7316742339663,56.0679277164066,-7.75677125828634)) ;
#3742 = CARTESIAN_POINT('',(164.931674233965,60.5679277164066,21.7432287417132)) ;
#3743 = CARTESIAN_POINT('',(130.931674233964,66.2679277164062,66.2432287417219)) ;
#3744 = UNCERTAINTY_MEASURE_WITH_UNIT(LENGTH_MEASURE(0.001),#3760,
'DISTANCE_ACCURACY_VALUE',
'Maximum model space distance between geometric entities at asserted c
onnectivities') ;
#3745 = UNCERTAINTY_MEASURE_WITH_UNIT(LENGTH_MEASURE(0.001),#3760,
'DISTANCE_ACCURACY_VALUE',
'Maximum model space distance between geometric entities at asserted c
onnectivities') ;
#3746 = UNCERTAINTY_MEASURE_WITH_UNIT(LENGTH_MEASURE(0.001),#3760,
'DISTANCE_ACCURACY_VALUE',
'Maximum model space distance between geometric entities at asserted c
onnectivities') ;
#3747 = UNCERTAINTY_MEASURE_WITH_UNIT(LENGTH_MEASURE(0.001),#3760,
'DISTANCE_ACCURACY_VALUE',
'Maximum model space distance between geometric entities at asserted c
onnectivities') ;
#3748 = UNCERTAINTY_MEASURE_WITH_UNIT(LENGTH_MEASURE(0.001),#3760,
'DISTANCE_ACCURACY_VALUE',
'Maximum model space distance between geometric entities at asserted c
onnectivities') ;
#3749 = UNCERTAINTY_MEASURE_WITH_UNIT(LENGTH_MEASURE(0.001),#3760,
'DISTANCE_ACCURACY_VALUE',
'Maximum model space distance between geometric entities at asserted c
onnectivities') ;
#3750 = UNCERTAINTY_MEASURE_WITH_UNIT(LENGTH_MEASURE(0.001),#3760,
'DISTANCE_ACCURACY_VALUE',
'Maximum model space distance between geometric entities at asserted c
onnectivities') ;
#3751 = UNCERTAINTY_MEASURE_WITH_UNIT(LENGTH_MEASURE(0.001),#3760,
'DISTANCE_ACCURACY_VALUE',
'Maximum model space distance between geometric entities at asserted c
onnectivities') ;
#3752 = (
GEOMETRIC_REPRESENTATION_CONTEXT(3)
GLOBAL_UNCERTAINTY_ASSIGNED_CONTEXT((#3744))
GLOBAL_UNIT_ASSIGNED_CONTEXT((#3760,#3762,#3763))
REPRESENTATION_CONTEXT('','3D')
) ;
#3753 = (
GEOMETRIC_REPRESENTATION_CONTEXT(3)
GLOBAL_UNCERTAINTY_ASSIGNED_CONTEXT((#3745))
GLOBAL_UNIT_ASSIGNED_CONTEXT((#3760,#3762,#3763))
REPRESENTATION_CONTEXT('','3D')
) ;
#3754 = (
GEOMETRIC_REPRESENTATION_CONTEXT(3)
GLOBAL_UNCERTAINTY_ASSIGNED_CONTEXT((#3746))
GLOBAL_UNIT_ASSIGNED_CONTEXT((#3760,#3762,#3763))
REPRESENTATION_CONTEXT('','3D')
) ;
#3755 = (
GEOMETRIC_REPRESENTATION_CONTEXT(3)
GLOBAL_UNCERTAINTY_ASSIGNED_CONTEXT((#3747))
GLOBAL_UNIT_ASSIGNED_CONTEXT((#3760,#3762,#3763))
REPRESENTATION_CONTEXT('','3D')
) ;
#3756 = (
GEOMETRIC_REPRESENTATION_CONTEXT(3)
GLOBAL_UNCERTAINTY_ASSIGNED_CONTEXT((#3748))
GLOBAL_UNIT_ASSIGNED_CONTEXT((#3760,#3762,#3763))
REPRESENTATION_CONTEXT('','3D')
) ;
#3757 = (
GEOMETRIC_REPRESENTATION_CONTEXT(3)
GLOBAL_UNCERTAINTY_ASSIGNED_CONTEXT((#3749))
GLOBAL_UNIT_ASSIGNED_CONTEXT((#3760,#3762,#3763))
REPRESENTATION_CONTEXT('','3D')
) ;
#3758 = (
GEOMETRIC_REPRESENTATION_CONTEXT(3)
GLOBAL_UNCERTAINTY_ASSIGNED_CONTEXT((#3750))
GLOBAL_UNIT_ASSIGNED_CONTEXT((#3760,#3762,#3763))
REPRESENTATION_CONTEXT('','3D')
) ;
#3759 = (
GEOMETRIC_REPRESENTATION_CONTEXT(3)
GLOBAL_UNCERTAINTY_ASSIGNED_CONTEXT((#3751))
GLOBAL_UNIT_ASSIGNED_CONTEXT((#3760,#3762,#3763))
REPRESENTATION_CONTEXT('','3D')
) ;
#3760 = (
LENGTH_UNIT()
NAMED_UNIT(*)
SI_UNIT(.CENTI.,.METRE.)
) ;
#3761 = (
LENGTH_UNIT()
NAMED_UNIT(*)
SI_UNIT($,.METRE.)
) ;
#3762 = (
NAMED_UNIT(*)
PLANE_ANGLE_UNIT()
SI_UNIT($,.RADIAN.)
) ;
#3763 = (
NAMED_UNIT(*)
SI_UNIT($,.STERADIAN.)
SOLID_ANGLE_UNIT()
) ;
#3764 = SHAPE_DEFINITION_REPRESENTATION(#3771,#3787) ;
#3765 = SHAPE_DEFINITION_REPRESENTATION(#3772,#3788) ;
#3766 = SHAPE_DEFINITION_REPRESENTATION(#3773,#3789) ;
#3767 = SHAPE_DEFINITION_REPRESENTATION(#3774,#3790) ;
#3768 = SHAPE_DEFINITION_REPRESENTATION(#3775,#3791) ;
#3769 = SHAPE_DEFINITION_REPRESENTATION(#3776,#3792) ;
#3770 = SHAPE_DEFINITION_REPRESENTATION(#3777,#3793) ;
#3771 = PRODUCT_DEFINITION_SHAPE('',$,#3795) ;
#3772 = PRODUCT_DEFINITION_SHAPE('',$,#3796) ;
#3773 = PRODUCT_DEFINITION_SHAPE('',$,#3797) ;
#3774 = PRODUCT_DEFINITION_SHAPE('',$,#3798) ;
#3775 = PRODUCT_DEFINITION_SHAPE('',$,#3799) ;
#3776 = PRODUCT_DEFINITION_SHAPE('',$,#3800) ;
#3777 = PRODUCT_DEFINITION_SHAPE('',$,#3801) ;
#3778 = PRODUCT_DEFINITION_SHAPE($,$,#38) ;
#3779 = PRODUCT_DEFINITION_SHAPE($,$,#39) ;
#3780 = PRODUCT_DEFINITION_SHAPE($,$,#40) ;
#3781 = PRODUCT_DEFINITION_SHAPE($,$,#41) ;
#3782 = PRODUCT_DEFINITION_SHAPE($,$,#42) ;
#3783 = PRODUCT_DEFINITION_SHAPE($,$,#43) ;
#3784 = PRODUCT_DEFINITION_SHAPE($,$,#44) ;
#3785 = PRODUCT_DEFINITION_SHAPE($,$,#45) ;
#3786 = PRODUCT_DEFINITION_SHAPE($,$,#46) ;
#3787 = SHAPE_REPRESENTATION('',(#2336,#2495,#2496,#2497,#2498,#2499,#2500,
#2501,#2502,#2503),#3752) ;
#3788 = SHAPE_REPRESENTATION('',(#2337),#3753) ;
#3789 = SHAPE_REPRESENTATION('',(#2369),#3754) ;
#3790 = SHAPE_REPRESENTATION('',(#2401),#3755) ;
#3791 = SHAPE_REPRESENTATION('',(#2429),#3756) ;
#3792 = SHAPE_REPRESENTATION('',(#2453),#3757) ;
#3793 = SHAPE_REPRESENTATION('',(#2474),#3758) ;
#3794 = PRODUCT_DEFINITION_CONTEXT('part definition',#3817,'design') ;
#3795 = PRODUCT_DEFINITION('MAS-635','MAS-635',#3802,#3794) ;
#3796 = PRODUCT_DEFINITION('Panel_Top_Front','Panel_Top_Front',
#3803,#3794) ;
#3797 = PRODUCT_DEFINITION('Panel_Top_Side_Inner',
'Panel_Top_Side_Inner',#3804,#3794) ;
#3798 = PRODUCT_DEFINITION('Panel_Top_Side_Outer',
'Panel_Top_Side_Outer',#3805,#3794) ;
#3799 = PRODUCT_DEFINITION('Panel_Top_Cap','Panel_Top_Cap',#3806,
#3794) ;
#3800 = PRODUCT_DEFINITION('Flange_Large','Flange_Large',#3807,
#3794) ;
#3801 = PRODUCT_DEFINITION('Flange_Small','Flange_Small',#3808,
#3794) ;
#3802 = PRODUCT_DEFINITION_FORMATION('',$,#3819) ;
#3803 = PRODUCT_DEFINITION_FORMATION('',$,#3820) ;
#3804 = PRODUCT_DEFINITION_FORMATION('',$,#3821) ;
#3805 = PRODUCT_DEFINITION_FORMATION('',$,#3822) ;
#3806 = PRODUCT_DEFINITION_FORMATION('',$,#3823) ;
#3807 = PRODUCT_DEFINITION_FORMATION('',$,#3824) ;
#3808 = PRODUCT_DEFINITION_FORMATION('',$,#3825) ;
#3809 = PRODUCT_RELATED_PRODUCT_CATEGORY('MAS-635','MAS-635',(#3819)) ;
#3810 = PRODUCT_RELATED_PRODUCT_CATEGORY('Panel_Top_Front',
'Panel_Top_Front',(#3820)) ;
#3811 = PRODUCT_RELATED_PRODUCT_CATEGORY('Panel_Top_Side_Inner',
'Panel_Top_Side_Inner',(#3821)) ;
#3812 = PRODUCT_RELATED_PRODUCT_CATEGORY('Panel_Top_Side_Outer',
'Panel_Top_Side_Outer',(#3822)) ;
#3813 = PRODUCT_RELATED_PRODUCT_CATEGORY('Panel_Top_Cap','Panel_Top_Cap',
(#3823)) ;
#3814 = PRODUCT_RELATED_PRODUCT_CATEGORY('Flange_Large','Flange_Large',(#3824)) ;
#3815 = PRODUCT_RELATED_PRODUCT_CATEGORY('Flange_Small','Flange_Small',(#3825)) ;
#3816 = APPLICATION_PROTOCOL_DEFINITION('international standard',
'automotive_design',2009,#3817) ;
#3817 = APPLICATION_CONTEXT(
'Core Data for Automotive Mechanical Design Process') ;
#3818 = PRODUCT_CONTEXT('part definition',#3817,'mechanical') ;
#3819 = PRODUCT('MAS-635','MAS-635','',(#3818)) ;
#3820 = PRODUCT('Panel_Top_Front','Panel_Top_Front',$,(#3818)) ;
#3821 = PRODUCT('Panel_Top_Side_Inner','Panel_Top_Side_Inner',$,(#3818)) ;
#3822 = PRODUCT('Panel_Top_Side_Outer','Panel_Top_Side_Outer',$,(#3818)) ;
#3823 = PRODUCT('Panel_Top_Cap','Panel_Top_Cap',$,(#3818)) ;
#3824 = PRODUCT('Flange_Large','Flange_Large',$,(#3818)) ;
#3825 = PRODUCT('Flange_Small','Flange_Small',$,(#3818)) ;
#3826 = PRESENTATION_STYLE_ASSIGNMENT((#3828)) ;
#3827 = PRESENTATION_STYLE_ASSIGNMENT((#3829)) ;
#3828 = SURFACE_STYLE_USAGE(.BOTH.,#3830) ;
#3829 = SURFACE_STYLE_USAGE(.BOTH.,#3831) ;
#3830 = SURFACE_SIDE_STYLE('',(#3832)) ;
#3831 = SURFACE_SIDE_STYLE('',(#3833)) ;
#3832 = SURFACE_STYLE_FILL_AREA(#3834) ;
#3833 = SURFACE_STYLE_FILL_AREA(#3835) ;
#3834 = FILL_AREA_STYLE('Steel - Satin',(#3836)) ;
#3835 = FILL_AREA_STYLE('Opaque(179,179,179)',(#3837)) ;
#3836 = FILL_AREA_STYLE_COLOUR('Steel - Satin',#3838) ;
#3837 = FILL_AREA_STYLE_COLOUR('Opaque(179,179,179)',#3839) ;
#3838 = COLOUR_RGB('Steel - Satin', 0.09019608, 0.27058824, 0.51372549) ;
#3839 = COLOUR_RGB('Opaque(179,179,179)', 0.09019608, 0.27058824, 0.51372549) ;
ENDSEC;
END-ISO-10303-21;
